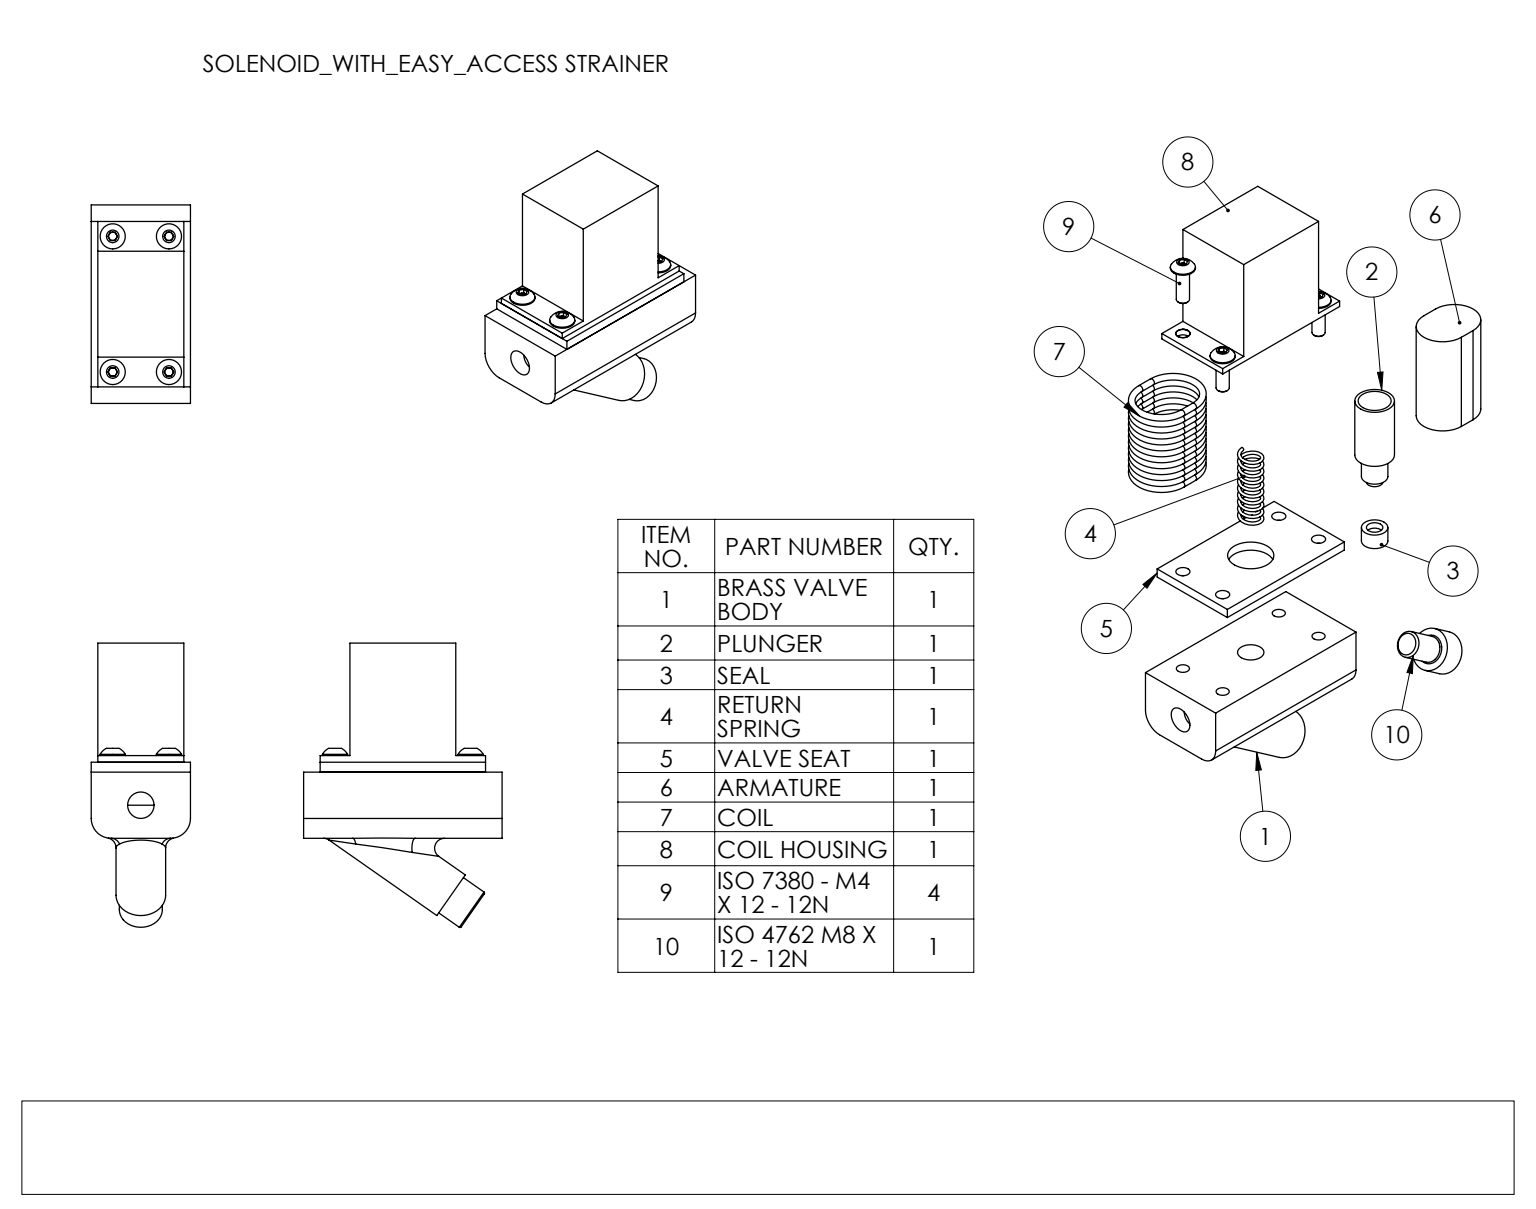
ISO-10303-21;
HEADER;
FILE_DESCRIPTION (('STEP AP214'),
    '1' );
FILE_NAME ('MAS-178',
    '2026-10-25T16:39:07',
    ( '' ),
    ( '' ),
    'SwSTEP 2.0',
    'SolidWorks 2026',
    '' );
FILE_SCHEMA (( 'AUTOMOTIVE_DESIGN' ));
ENDSEC;

DATA;
#1 = CARTESIAN_POINT ( 'NONE',  ( 1.444289557195957086, 32.75319992234354061, -4.262301884875733471 ) ) ;
#2 = CARTESIAN_POINT ( 'NONE',  ( 2.000000000000004441, -20.45500799277048287, -10.97077568596606056 ) ) ;
#3 = EDGE_LOOP ( 'NONE', ( #1646, #9949, #917, #16022, #4902 ) ) ;
#4 = CIRCLE ( 'NONE', #8561, 2.499999999999999556 ) ;
#5 = DIRECTION ( 'NONE',  ( -0.000000000000000000, 1.000000000000000000, -0.000000000000000000 ) ) ;
#6 = CARTESIAN_POINT ( 'NONE',  ( 3.518350579753631191, 24.37180007765648071, 1.080741659609802285 ) ) ;
#7 = CARTESIAN_POINT ( 'NONE',  ( 9.986002763741593569, -9.918550557884699970, 7.302443594976057106 ) ) ;
#8 = CARTESIAN_POINT ( 'NONE',  ( 2.121784821875004390, -19.91118585227123816, -10.56187548683408828 ) ) ;
#9 = CARTESIAN_POINT ( 'NONE',  ( -1.336863392178478716, 22.49680007765647360, 4.297206761780677731 ) ) ;
#10 = CARTESIAN_POINT ( 'NONE',  ( 3.579096709490575479E-14, -22.86967407583208711, -1.406012196336041020 ) ) ;
#11 = LINE ( 'NONE', #8170, #4109 ) ;
#12 = ORIENTED_EDGE ( 'NONE', *, *, #11357, .T. ) ;
#13 = VERTEX_POINT ( 'NONE', #16013 ) ;
#14 = CARTESIAN_POINT ( 'NONE',  ( -2.115076519116362519, 25.12180007765647360, 3.012182706137107147 ) ) ;
#15 = EDGE_CURVE ( 'NONE', #13968, #17116, #3305, .T. ) ;
#16 = FACE_OUTER_BOUND ( 'NONE', #9142, .T. ) ;
#17 = CARTESIAN_POINT ( 'NONE',  ( 0.000000000000000000, 0.000000000000000000, 4.000000000000000000 ) ) ;
#18 = FACE_OUTER_BOUND ( 'NONE', #18196, .T. ) ;
#19 = EDGE_LOOP ( 'NONE', ( #11268, #10681 ) ) ;
#20 = AXIS2_PLACEMENT_3D ( 'NONE', #7890, #15986, #13371 ) ;
#21 = CARTESIAN_POINT ( 'NONE',  ( 3.518350579753605434, 18.12819992234353705, -1.080741659609877114 ) ) ;
#22 = CARTESIAN_POINT ( 'NONE',  ( 4.243569643750000786, -23.22272928460757413, -8.884014471503119736 ) ) ;
#23 = CARTESIAN_POINT ( 'NONE',  ( -2.798362969681365886, 35.24680007765648071, 2.102939460078824929 ) ) ;
#24 = CARTESIAN_POINT ( 'NONE',  ( 0.05938372350920109732, 27.62819992234353705, -3.680117784833935701 ) ) ;
#25 = DIRECTION ( 'NONE',  ( 0.000000000000000000, 0.000000000000000000, -1.000000000000000000 ) ) ;
#26 = CYLINDRICAL_SURFACE ( 'NONE', #5055, 6.500000000000000000 ) ;
#27 = CARTESIAN_POINT ( 'NONE',  ( -5.330712181944245322E-15, -26.55907985683728967, -5.105836667743160362 ) ) ;
#28 = CIRCLE ( 'NONE', #5350, 0.9999999999999991118 ) ;
#29 = CARTESIAN_POINT ( 'NONE',  ( 10.00000000000000355, 23.19999999999999574, 2.499999999999996891 ) ) ;
#30 = ADVANCED_FACE ( 'NONE', ( #12002 ), #4961, .F. ) ;
#31 = EDGE_CURVE ( 'NONE', #634, #10845, #10430, .T. ) ;
#32 = DIRECTION ( 'NONE',  ( 1.000000000000000000, 0.000000000000000000, 0.000000000000000000 ) ) ;
#33 = ADVANCED_FACE ( 'NONE', ( #17875 ), #13949, .T. ) ;
#34 = DIRECTION ( 'NONE',  ( -0.000000000000000000, -1.000000000000000000, -0.000000000000000000 ) ) ;
#35 = CARTESIAN_POINT ( 'NONE',  ( -4.243569643750000786, -19.99636183013295820, -4.276284222377527477 ) ) ;
#36 = DIRECTION ( 'NONE',  ( 0.000000000000000000, 0.000000000000000000, 1.000000000000000000 ) ) ;
#37 = SURFACE_STYLE_USAGE ( .BOTH. , #13947 ) ;
#38 = ORIENTED_EDGE ( 'NONE', *, *, #726, .T. ) ;
#39 = CARTESIAN_POINT ( 'NONE',  ( -2.518350579753611207, 21.87819992234354416, 0.7558219633769609480 ) ) ;
#40 = CYLINDRICAL_SURFACE ( 'NONE', #15087, 5.000000000000000000 ) ;
#41 = CARTESIAN_POINT ( 'NONE',  ( -11.99999999999999822, 48.00000000000000000, 15.00000000000000000 ) ) ;
#42 = STYLED_ITEM ( 'NONE', ( #4855 ), #12463 ) ;
#43 = FACE_OUTER_BOUND ( 'NONE', #17351, .T. ) ;
#44 = LINE ( 'NONE', #5782, #7268 ) ;
#45 = ORIENTED_EDGE ( 'NONE', *, *, #5518, .T. ) ;
#46 = CARTESIAN_POINT ( 'NONE',  ( -4.243569643750000786, -20.54484429739364515, -5.059598364728879361 ) ) ;
#47 = CARTESIAN_POINT ( 'NONE',  ( 0.05938372350927906274, 32.37180007765647360, 3.680117784833935701 ) ) ;
#48 = DIRECTION ( 'NONE',  ( 0.000000000000000000, 0.000000000000000000, -1.000000000000000000 ) ) ;
#49 = CARTESIAN_POINT ( 'NONE',  ( -2.121784821874996396, -23.22358977219849407, -15.29247854260303718 ) ) ;
#50 =( BOUNDED_CURVE ( )  B_SPLINE_CURVE ( 2, ( #611, #13389, #3391, #8936, #1817, #3112, #11902, #16101, #955 ),
 .UNSPECIFIED., .F., .F. ) 
 B_SPLINE_CURVE_WITH_KNOTS ( ( 3, 2, 2, 2, 3 ),
 ( 0.3879310344827586188, 0.3908045977011494476, 0.3965517241379310498, 0.4022988505747126520, 0.4051724137931034808 ),
 .UNSPECIFIED. ) 
 CURVE ( )  GEOMETRIC_REPRESENTATION_ITEM ( )  RATIONAL_B_SPLINE_CURVE ( ( 0.9330127018922194093, 0.9330127018922194093, 1.000000000000000000, 0.8660254037844387076, 1.000000000000000000, 0.8660254037844387076, 1.000000000000000000, 0.9330127018922187432, 0.9330127018922194093 ) ) 
 REPRESENTATION_ITEM ( '' )  );
#51 = DIRECTION ( 'NONE',  ( 1.000000000000000000, 0.000000000000000000, -4.336808689942021680E-16 ) ) ;
#52 = PRESENTATION_LAYER_ASSIGNMENT (  '', '', ( #2717 ) ) ;
#53 = DIRECTION ( 'NONE',  ( -0.000000000000000000, -0.5735764363510414965, -0.8191520442889950182 ) ) ;
#54 = CARTESIAN_POINT ( 'NONE',  ( 4.243569643750003451, -22.48482328119956009, -12.10166559521431573 ) ) ;
#55 = ORIENTED_EDGE ( 'NONE', *, *, #17293, .T. ) ;
#56 = DIRECTION ( 'NONE',  ( -3.373073425510457965E-16, 0.000000000000000000, -1.000000000000000000 ) ) ;
#57 = CARTESIAN_POINT ( 'NONE',  ( -1.999999999999996225, -18.15353254261686899, -7.683928109263233885 ) ) ;
#58 = CARTESIAN_POINT ( 'NONE',  ( 2.055738996568313048, 21.99680007765648426, 1.423772053676023441 ) ) ;
#59 = EDGE_LOOP ( 'NONE', ( #6650, #2880, #2585, #4940 ) ) ;
#60 = DIRECTION ( 'NONE',  ( -1.000000000000000000, 0.000000000000000000, 4.336808689942021680E-16 ) ) ;
#61 = VECTOR ( 'NONE', #15535, 1000.000000000000000 ) ;
#62 = EDGE_CURVE ( 'NONE', #4590, #2518, #8726, .T. ) ;
#63 = AXIS2_PLACEMENT_3D ( 'NONE', #11586, #12802, #2984 ) ;
#64 = CARTESIAN_POINT ( 'NONE',  ( 3.999999999999996447, -25.24891187463481046, -7.751385191667569785 ) ) ;
#65 = CARTESIAN_POINT ( 'NONE',  ( 0.8262555684460829442, 37.75319992234354771, -2.360188852285421302 ) ) ;
#66 = EDGE_LOOP ( 'NONE', ( #4791, #2042, #17064, #10532, #9168 ) ) ;
#67 = CARTESIAN_POINT ( 'NONE',  ( 2.121784821875004390, -20.71777771588989125, -11.71380804911548701 ) ) ;
#68 = CARTESIAN_POINT ( 'NONE',  ( -4.000000000000000888, -26.36843755307278414, -13.37655146490396341 ) ) ;
#69 = CARTESIAN_POINT ( 'NONE',  ( 4.518350579753633411, 31.87180007765647716, 1.405661355842698468 ) ) ;
#70 = EDGE_LOOP ( 'NONE', ( #14455, #11089, #12235, #9427, #6688 ) ) ;
#71 = DIRECTION ( 'NONE',  ( 1.000000000000000000, 0.000000000000000000, 0.000000000000000000 ) ) ;
#72 = CARTESIAN_POINT ( 'NONE',  ( 1.071796769724485232, -23.37436616782919074, -2.126787201540221162 ) ) ;
#73 = DIRECTION ( 'NONE',  ( -0.000000000000000000, 1.000000000000000000, -0.000000000000000000 ) ) ;
#74 = AXIS2_PLACEMENT_3D ( 'NONE', #11287, #9899, #17353 ) ;
#75 = DIRECTION ( 'NONE',  ( -0.000000000000000000, 1.000000000000000000, -0.000000000000000000 ) ) ;
#76 =( GEOMETRIC_REPRESENTATION_CONTEXT ( 3 ) GLOBAL_UNCERTAINTY_ASSIGNED_CONTEXT ( ( #9698 ) ) GLOBAL_UNIT_ASSIGNED_CONTEXT ( ( #9720, #5466, #12594 ) ) REPRESENTATION_CONTEXT ( 'NONE', 'WORKASPACE' ) );
#77 = CARTESIAN_POINT ( 'NONE',  ( 10.00000000000000000, 34.19999999999999574, -2.500000000000003109 ) ) ;
#78 = CARTESIAN_POINT ( 'NONE',  ( 4.243569643749996345, -23.73478956620236957, -5.343822230353133307 ) ) ;
#79 = ADVANCED_FACE ( 'NONE', ( #10984 ), #15448, .F. ) ;
#80 = ORIENTED_EDGE ( 'NONE', *, *, #14785, .F. ) ;
#81 = CARTESIAN_POINT ( 'NONE',  ( 3.885274725274725949, -4.336808689942017736E-16, 0.000000000000000000 ) ) ;
#82 = ORIENTED_EDGE ( 'NONE', *, *, #14672, .T. ) ;
#83 = ORIENTED_EDGE ( 'NONE', *, *, #13971, .F. ) ;
#84 = DIRECTION ( 'NONE',  ( -0.000000000000000000, 1.000000000000000000, -0.000000000000000000 ) ) ;
#85 = EDGE_CURVE ( 'NONE', #1006, #3919, #10004, .T. ) ;
#86 = LINE ( 'NONE', #7211, #12515 ) ;
#87 = CARTESIAN_POINT ( 'NONE',  ( 4.499999999999999112, 18.25319992234354771, 0.05647727720528474687 ) ) ;
#88 = CARTESIAN_POINT ( 'NONE',  ( -2.115076519116425580, 27.37819992234354771, -3.012182706137063182 ) ) ;
#89 = CARTESIAN_POINT ( 'NONE',  ( 3.999999999999996447, -27.63642379165096941, -11.16110557702727668 ) ) ;
#90 = CARTESIAN_POINT ( 'NONE',  ( -1.593127413382998459, 35.87180007765648071, -2.091722143975139669 ) ) ;
#91 = AXIS2_PLACEMENT_3D ( 'NONE', #15450, #198, #8713 ) ;
#92 = CARTESIAN_POINT ( 'NONE',  ( 2.733110507866328920, 36.12819992234354771, 3.862833514489095510 ) ) ;
#93 = CARTESIAN_POINT ( 'NONE',  ( 1.999999999999994449, -26.47440569391090648, -7.488412793402255296 ) ) ;
#94 = VERTEX_POINT ( 'NONE', #4123 ) ;
#95 = CARTESIAN_POINT ( 'NONE',  ( 0.000000000000000000, 5.977523610840987267, 32.81826849749789687 ) ) ;
#96 = CARTESIAN_POINT ( 'NONE',  ( 2.798362969681366330, 18.99680007765648071, -2.102939460078824929 ) ) ;
#97 = CARTESIAN_POINT ( 'NONE',  ( 9.570744302495992173, -9.974069202854233041, -0.5947597794661263482 ) ) ;
#98 = CARTESIAN_POINT ( 'NONE',  ( -4.243569643749998122, -21.36634923031502353, -10.50431910885077791 ) ) ;
#99 = CARTESIAN_POINT ( 'NONE',  ( 4.518350579753633411, 21.87180007765647360, 1.405661355842698468 ) ) ;
#100 = AXIS2_PLACEMENT_3D ( 'NONE', #14724, #10710, #2117 ) ;
#101 = CARTESIAN_POINT ( 'NONE',  ( 1.071796769724504328, -22.85814737511324424, -1.389550361680131685 ) ) ;
#102 = CARTESIAN_POINT ( 'NONE',  ( 4.000000000000000888, -19.98022999250811793, -4.253245570628513939 ) ) ;
#103 = EDGE_CURVE ( 'NONE', #5353, #12502, #9927, .T. ) ;
#104 = ORIENTED_EDGE ( 'NONE', *, *, #5539, .F. ) ;
#105 = EDGE_LOOP ( 'NONE', ( #9337, #11121, #10529, #10635, #17849 ) ) ;
#106 = CARTESIAN_POINT ( 'NONE',  ( -3.500000000000000444, 22.99680007765647716, 0.05647727720536892260 ) ) ;
#107 = CARTESIAN_POINT ( 'NONE',  ( 0.000000000000000000, 29.79999999999999716, 2.500000000000000000 ) ) ;
#108 = CYLINDRICAL_SURFACE ( 'NONE', #4806, 0.9999999999999991118 ) ;
#109 =( LENGTH_UNIT ( ) NAMED_UNIT ( * ) SI_UNIT ( .MILLI., .METRE. ) );
#110 = EDGE_LOOP ( 'NONE', ( #10063, #7100, #15621, #8878 ) ) ;
#111 = CARTESIAN_POINT ( 'NONE',  ( -3.481649420246394122, 22.12819992234353705, -1.193696214020467883 ) ) ;
#112 = CARTESIAN_POINT ( 'NONE',  ( 4.243569643750000786, -23.48083868096554028, -9.252632891433169249 ) ) ;
#113 = CARTESIAN_POINT ( 'NONE',  ( 2.211161402132902243, 37.12180007765645939, 2.942372952327172442 ) ) ;
#114 = CARTESIAN_POINT ( 'NONE',  ( 1.027846397803612311, 36.25319992234354771, 3.346150245485499219 ) ) ;
#115 = CARTESIAN_POINT ( 'NONE',  ( 1.300000000000000044, -1.443375672974064328, 2.168404344971008868E-16 ) ) ;
#116 = CARTESIAN_POINT ( 'NONE',  ( 4.898587196589413815E-16, 2.700915433685006750, 35.11257424290206330 ) ) ;
#117 = VECTOR ( 'NONE', #8182, 1000.000000000000000 ) ;
#118 = CARTESIAN_POINT ( 'NONE',  ( -2.121784821874996396, -19.38421250137371388, -9.809279546143578443 ) ) ;
#119 = CARTESIAN_POINT ( 'NONE',  ( -2.526502195916607629, -15.31622431266957207, -9.916727303590223030 ) ) ;
#120 = CARTESIAN_POINT ( 'NONE',  ( -5.577813053751546416E-15, -24.16022105762193206, -3.249104295986281699 ) ) ;
#121 = CARTESIAN_POINT ( 'NONE',  ( 8.500000000000001776, 13.00000000000000178, -20.49999999999999645 ) ) ;
#122 = CARTESIAN_POINT ( 'NONE',  ( 4.243569643749996345, -22.92819770258371292, -4.191889668071731911 ) ) ;
#123 = CARTESIAN_POINT ( 'NONE',  ( 1.071796769724485454, -21.36111765121935235, -13.19914471043622228 ) ) ;
#124 =( NAMED_UNIT ( * ) SI_UNIT ( $, .STERADIAN. ) SOLID_ANGLE_UNIT ( ) );
#125 = ORIENTED_EDGE ( 'NONE', *, *, #9998, .T. ) ;
#126 = CARTESIAN_POINT ( 'NONE',  ( -0.05938372350921170689, 21.37819992234354416, 2.628655560595669183 ) ) ;
#127 = CARTESIAN_POINT ( 'NONE',  ( -5.577813053751546416E-15, -25.38624068961733826, -5.000041789647243107 ) ) ;
#128 = DIRECTION ( 'NONE',  ( -1.000000000000000000, -0.000000000000000000, -0.000000000000000000 ) ) ;
#129 = CYLINDRICAL_SURFACE ( 'NONE', #10158, 6.000000000000000000 ) ;
#130 = DIRECTION ( 'NONE',  ( -1.000000000000000000, 0.000000000000000000, -0.000000000000000000 ) ) ;
#131 = EDGE_CURVE ( 'NONE', #9627, #9963, #4373, .T. ) ;
#132 = ORIENTED_EDGE ( 'NONE', *, *, #13174, .F. ) ;
#133 = CARTESIAN_POINT ( 'NONE',  ( 2.121784821875004390, -17.62046495959427261, -7.290387009954915953 ) ) ;
#134 = CARTESIAN_POINT ( 'NONE',  ( -0.05938372350927861171, 36.12180007765648782, -3.680117784833935701 ) ) ;
#135 = CARTESIAN_POINT ( 'NONE',  ( -4.000000000000000888, -19.85117529432912775, -4.068936360663492735 ) ) ;
#136 = ADVANCED_FACE ( 'NONE', ( #2566 ), #16663, .T. ) ;
#137 = EDGE_CURVE ( 'NONE', #3649, #894, #1162, .T. ) ;
#138 = CARTESIAN_POINT ( 'NONE',  ( -4.243569643749998122, -23.17311500482080433, -13.08464804836111206 ) ) ;
#139 = CARTESIAN_POINT ( 'NONE',  ( 9.000000000000005329, 36.39999999999999147, 2.499999999999997335 ) ) ;
#140 = VECTOR ( 'NONE', #8743, 1000.000000000000000 ) ;
#141 = EDGE_CURVE ( 'NONE', #15889, #18202, #16275, .T. ) ;
#142 = DIRECTION ( 'NONE',  ( 0.000000000000000000, 0.000000000000000000, -1.000000000000000000 ) ) ;
#143 = LINE ( 'NONE', #14051, #16513 ) ;
#144 = CARTESIAN_POINT ( 'NONE',  ( 4.243569643749996345, -26.79983864795324422, -9.721165967022450616 ) ) ;
#145 = LINE ( 'NONE', #7551, #15141 ) ;
#146 = CARTESIAN_POINT ( 'NONE',  ( -1.999999999999996225, -17.37920435354295989, -6.578072849473089789 ) ) ;
#147 = CARTESIAN_POINT ( 'NONE',  ( 1.593127413382998903, 24.62180007765647716, 2.091722143975139669 ) ) ;
#148 = ORIENTED_EDGE ( 'NONE', *, *, #10556, .T. ) ;
#149 = CARTESIAN_POINT ( 'NONE',  ( 2.115076519116362963, 23.87180007765647360, -3.012182706137107591 ) ) ;
#150 = EDGE_CURVE ( 'NONE', #12707, #13230, #14438, .T. ) ;
#151 = CARTESIAN_POINT ( 'NONE',  ( 0.000000000000000000, 5.977523610840987267, 32.81826849749789687 ) ) ;
#152 = CARTESIAN_POINT ( 'NONE',  ( 0.000000000000000000, 0.000000000000000000, 0.000000000000000000 ) ) ;
#153 = DIRECTION ( 'NONE',  ( 0.000000000000000000, 0.000000000000000000, 1.000000000000000000 ) ) ;
#154 = CARTESIAN_POINT ( 'NONE',  ( -0.05938372350921170689, 33.87819992234354061, 2.628655560595669183 ) ) ;
#155 = PRODUCT_DEFINITION ( 'UNKNOWN', '', #10424, #5149 ) ;
#156 = VERTEX_POINT ( 'NONE', #15172 ) ;
#157 = CARTESIAN_POINT ( 'NONE',  ( -2.121784821874996396, -21.44908767223746437, -12.75822690558396033 ) ) ;
#158 = CARTESIAN_POINT ( 'NONE',  ( -3.607379964056306676, 35.24680007765647360, 2.690724712371306282 ) ) ;
#159 = VERTEX_POINT ( 'NONE', #2476 ) ;
#160 = VECTOR ( 'NONE', #10107, 1000.000000000000000 ) ;
#161 = CARTESIAN_POINT ( 'NONE',  ( 3.999999999999995559, 2.343145750507624747, 2.343145750507618086 ) ) ;
#162 = CARTESIAN_POINT ( 'NONE',  ( -5.577813053751546416E-15, -26.16056887869124381, -6.105897049437384538 ) ) ;
#163 = CARTESIAN_POINT ( 'NONE',  ( 1.071796769724485232, -25.37471398889850605, -4.983579954991325778 ) ) ;
#164 = CARTESIAN_POINT ( 'NONE',  ( -5.577813053751546416E-15, -29.06429958842333505, -10.25285427465718868 ) ) ;
#165 = LINE ( 'NONE', #4426, #8792 ) ;
#166 = CARTESIAN_POINT ( 'NONE',  ( 2.121784821874994176, -23.98544242790896774, -3.566046559362932467 ) ) ;
#167 = ORIENTED_EDGE ( 'NONE', *, *, #2613, .T. ) ;
#168 = CARTESIAN_POINT ( 'NONE',  ( 9.000000000000001776, 20.99999999999999289, -2.500000000000002665 ) ) ;
#169 = EDGE_LOOP ( 'NONE', ( #15590, #17525, #15025, #11757 ) ) ;
#170 = ORIENTED_EDGE ( 'NONE', *, *, #9208, .T. ) ;
#171 = CYLINDRICAL_SURFACE ( 'NONE', #7169, 2.000000000000001776 ) ;
#172 = LINE ( 'NONE', #7581, #17268 ) ;
#173 = CARTESIAN_POINT ( 'NONE',  ( 2.733110507866328920, 21.12819992234354416, 3.862833514489095510 ) ) ;
#174 = CARTESIAN_POINT ( 'NONE',  ( -2.211161402132838738, 26.62819992234354416, 2.942372952327218183 ) ) ;
#175 = AXIS2_PLACEMENT_3D ( 'NONE', #15900, #11338, #4486 ) ;
#176 = CARTESIAN_POINT ( 'NONE',  ( -1.989345975306426206, 40.24680007765648071, 1.515154207786343799 ) ) ;
#177 = VERTEX_POINT ( 'NONE', #8106 ) ;
#178 = CARTESIAN_POINT ( 'NONE',  ( 0.05938372350919016857, 32.62819992234354771, -4.731580009072201776 ) ) ;
#179 = CARTESIAN_POINT ( 'NONE',  ( -3.999999999999997335, -21.07824655387797819, -9.847693641197304615 ) ) ;
#180 = ORIENTED_EDGE ( 'NONE', *, *, #14181, .F. ) ;
#181 = DIRECTION ( 'NONE',  ( 1.000000000000000000, 0.000000000000000000, 0.000000000000000000 ) ) ;
#182 = CARTESIAN_POINT ( 'NONE',  ( -2.798362969681365886, 30.24680007765648071, 2.102939460078824929 ) ) ;
#183 = CLOSED_SHELL ( 'NONE', ( #8623, #12070, #5801, #4336, #16789, #13518, #7804, #15959, #10685, #12852, #17802, #16024, #17150, #1736, #8963, #16034, #14996, #8741, #15227, #15885, #6061, #555, #6136, #15606, #14685, #7463, #6386 ) ) ;
#184 = CARTESIAN_POINT ( 'NONE',  ( -9.604277560388482016, -9.971758527880211886, 12.06915245473052778 ) ) ;
#185 = CARTESIAN_POINT ( 'NONE',  ( 4.243569643750003451, -19.90372931761987019, -8.415481395913838369 ) ) ;
#186 = CIRCLE ( 'NONE', #5222, 0.9999999999999991118 ) ;
#187 = CARTESIAN_POINT ( 'NONE',  ( 4.518350579753633411, 34.37180007765647360, 1.405661355842698468 ) ) ;
#188 = DIRECTION ( 'NONE',  ( -0.000000000000000000, -1.000000000000000000, -0.000000000000000000 ) ) ;
#189 = ORIENTED_EDGE ( 'NONE', *, *, #16096, .T. ) ;
#190 = ORIENTED_EDGE ( 'NONE', *, *, #1172, .T. ) ;
#191 = CARTESIAN_POINT ( 'NONE',  ( -2.115076519116362519, 27.62180007765648071, 3.012182706137107147 ) ) ;
#192 = CARTESIAN_POINT ( 'NONE',  ( 4.000000000000000000, 3.518949890710770134, -4.119968255444916849E-15 ) ) ;
#193 = DIRECTION ( 'NONE',  ( 0.000000000000000000, 0.000000000000000000, -1.000000000000000000 ) ) ;
#194 = CARTESIAN_POINT ( 'NONE',  ( 1.533898589781675205E-14, -27.70922525683905846, -8.317607569017670954 ) ) ;
#195 = FILL_AREA_STYLE ('',( #580 ) ) ;
#196 = VERTEX_POINT ( 'NONE', #13765 ) ;
#197 = CARTESIAN_POINT ( 'NONE',  ( 2.115076519116426024, 21.12819992234353705, 3.012182706137062294 ) ) ;
#198 = DIRECTION ( 'NONE',  ( -1.000000000000000000, -0.000000000000000000, -0.000000000000000000 ) ) ;
#199 = CARTESIAN_POINT ( 'NONE',  ( 4.730628863548789710E-15, -18.62809540513275408, -10.86517747810410306 ) ) ;
#200 = CARTESIAN_POINT ( 'NONE',  ( -3.481649420246369697, 37.87180007765648071, 1.193696214020542490 ) ) ;
#201 = EDGE_CURVE ( 'NONE', #2949, #3217, #16754, .T. ) ;
#202 = CARTESIAN_POINT ( 'NONE',  ( -0.05938372350920063936, 31.37819992234354416, 3.680117784833935701 ) ) ;
#203 = FACE_OUTER_BOUND ( 'NONE', #11493, .T. ) ;
#204 = VECTOR ( 'NONE', #11238, 1000.000000000000227 ) ;
#205 = DIRECTION ( 'NONE',  ( 0.000000000000000000, 0.8191520442889952403, -0.5735764363510413855 ) ) ;
#206 = CARTESIAN_POINT ( 'NONE',  ( -4.243569643750005227, -25.11137301344485451, -7.309787136646725081 ) ) ;
#207 = EDGE_CURVE ( 'NONE', #12141, #13551, #11942, .T. ) ;
#208 = CYLINDRICAL_SURFACE ( 'NONE', #2997, 2.000000000000001776 ) ;
#209 = PRODUCT_DEFINITION_CONTEXT ( 'detailed design', #4162, 'design' ) ;
#210 = EDGE_CURVE ( 'NONE', #16170, #12849, #15356, .T. ) ;
#211 = CARTESIAN_POINT ( 'NONE',  ( -4.371749249414769167, -10.00000000000000178, -10.94697576041360954 ) ) ;
#212 = DIRECTION ( 'NONE',  ( 0.000000000000000000, 0.8191520442889952403, -0.5735764363510413855 ) ) ;
#213 = DIRECTION ( 'NONE',  ( 1.000000000000000000, 0.000000000000000000, 0.000000000000000000 ) ) ;
#214 = VECTOR ( 'NONE', #7659, 1000.000000000000000 ) ;
#215 = CARTESIAN_POINT ( 'NONE',  ( 4.730628863548789710E-15, -16.82132963062697684, -8.284848538593767131 ) ) ;
#216 = CARTESIAN_POINT ( 'NONE',  ( -1.086818808809129289, 15.00000000000000533, -3.240250934315705322 ) ) ;
#217 = CARTESIAN_POINT ( 'NONE',  ( 2.000000000000004441, -17.68033198262726913, -7.008127672724814516 ) ) ;
#218 = VERTEX_POINT ( 'NONE', #12642 ) ;
#219 = CARTESIAN_POINT ( 'NONE',  ( 0.8262555684460829442, 20.25319992234354771, -2.360188852285421302 ) ) ;
#220 = CARTESIAN_POINT ( 'NONE',  ( 4.243569643749996345, -28.60660442245902146, -12.30149490653278121 ) ) ;
#221 = DIRECTION ( 'NONE',  ( -1.000000000000000000, 0.000000000000000000, 0.000000000000000000 ) ) ;
#222 = CARTESIAN_POINT ( 'NONE',  ( -1.444289557196047014, 18.49680007765647360, -4.262301884875704161 ) ) ;
#223 = CARTESIAN_POINT ( 'NONE',  ( -8.999999999999996447, -10.00000000000000000, 15.14468620625656925 ) ) ;
#224 = DIRECTION ( 'NONE',  ( -6.162975822039154730E-33, 0.5735764363510414965, 0.8191520442889950182 ) ) ;
#225 = ADVANCED_FACE ( 'NONE', ( #14226 ), #13254, .T. ) ;
#226 = CLOSED_SHELL ( 'NONE', ( #8070, #9759, #11243, #8369, #10714, #5967, #5501, #385, #7224, #136 ) ) ;
#227 = ORIENTED_EDGE ( 'NONE', *, *, #6831, .F. ) ;
#228 = CARTESIAN_POINT ( 'NONE',  ( 2.121784821875004390, -17.36235556323629936, -6.921768590024867329 ) ) ;
#229 = CARTESIAN_POINT ( 'NONE',  ( -0.05938372350927861171, 31.12180007765647005, -3.680117784833935701 ) ) ;
#230 = CARTESIAN_POINT ( 'NONE',  ( 3.064182432158234271, -21.85725826261086624, -2.451265441397198153 ) ) ;
#231 = AXIS2_PLACEMENT_3D ( 'NONE', #14903, #8098, #17958 ) ;
#232 = CARTESIAN_POINT ( 'NONE',  ( 9.000000000000005329, 23.19999999999999574, 2.499999999999997335 ) ) ;
#233 = CARTESIAN_POINT ( 'NONE',  ( 4.243569643749997233, -27.57416683702714622, -10.82702122681259205 ) ) ;
#234 = CARTESIAN_POINT ( 'NONE',  ( 3.061616997868382648E-16, 3.000000000000000000, -2.499999999999999556 ) ) ;
#235 = CYLINDRICAL_SURFACE ( 'NONE', #4146, 4.000000000000000000 ) ;
#236 = DIRECTION ( 'NONE',  ( 0.000000000000000000, 0.8191520442889952403, -0.5735764363510413855 ) ) ;
#237 = CARTESIAN_POINT ( 'NONE',  ( -4.243569643750000786, -24.64233096457639505, -10.91141578111838584 ) ) ;
#238 = EDGE_CURVE ( 'NONE', #14275, #456, #5568, .T. ) ;
#239 = PLANE ( 'NONE',  #7419 ) ;
#240 = CARTESIAN_POINT ( 'NONE',  ( -5.279047395330986450E-15, -24.40900471032784935, -2.525555542035599288 ) ) ;
#241 = AXIS2_PLACEMENT_3D ( 'NONE', #5032, #10687, #16359 ) ;
#242 = CARTESIAN_POINT ( 'NONE',  ( 2.518350579753628971, 21.87180007765647360, 0.7558219633769073242 ) ) ;
#243 = CIRCLE ( 'NONE', #11190, 2.149999999999999023 ) ;
#244 = VERTEX_POINT ( 'NONE', #11334 ) ;
#245 = CARTESIAN_POINT ( 'NONE',  ( 0.05938372350927906967, 19.87180007765648071, 3.680117784833935701 ) ) ;
#246 = FACE_OUTER_BOUND ( 'NONE', #4639, .T. ) ;
#247 = DIRECTION ( 'NONE',  ( 0.000000000000000000, -1.000000000000000000, 0.000000000000000000 ) ) ;
#248 = CARTESIAN_POINT ( 'NONE',  ( 1.071796769724504328, -26.66526097068834034, -6.826672054641570675 ) ) ;
#249 = CARTESIAN_POINT ( 'NONE',  ( 0.7188294034286553114, 33.75319992234354771, 2.395093729190349130 ) ) ;
#250 = ORIENTED_EDGE ( 'NONE', *, *, #10800, .T. ) ;
#251 = CARTESIAN_POINT ( 'NONE',  ( 2.121784821874994176, -27.34086458056255964, -8.358086018453551702 ) ) ;
#252 = CARTESIAN_POINT ( 'NONE',  ( -2.733110507866247652, 32.62180007765647360, 3.862833514489154574 ) ) ;
#253 = ORIENTED_EDGE ( 'NONE', *, *, #12378, .T. ) ;
#254 =( GEOMETRIC_REPRESENTATION_CONTEXT ( 3 ) GLOBAL_UNCERTAINTY_ASSIGNED_CONTEXT ( ( #16629 ) ) GLOBAL_UNIT_ASSIGNED_CONTEXT ( ( #17586, #16356, #4937 ) ) REPRESENTATION_CONTEXT ( 'NONE', 'WORKASPACE' ) );
#255 = TOROIDAL_SURFACE ( 'NONE', #10616, 9.000000000000001776, 0.9999999999999991118 ) ;
#256 = CARTESIAN_POINT ( 'NONE',  ( 7.960204194457794491E-16, 43.00000000000000000, 6.499999999999999112 ) ) ;
#257 = CARTESIAN_POINT ( 'NONE',  ( 4.243569643750003451, -23.54952454117618288, -13.62221657742576397 ) ) ;
#258 = DIRECTION ( 'NONE',  ( 0.000000000000000000, 0.000000000000000000, 1.000000000000000000 ) ) ;
#259 = CYLINDRICAL_SURFACE ( 'NONE', #5612, 4.000000000000000000 ) ;
#260 = DIRECTION ( 'NONE',  ( -0.000000000000000000, -1.000000000000000000, 1.502314598737159031E-16 ) ) ;
#261 = CARTESIAN_POINT ( 'NONE',  ( -4.243569643749997233, -19.84995652671195998, -8.338685891761748792 ) ) ;
#262 = ORIENTED_EDGE ( 'NONE', *, *, #17903, .F. ) ;
#263 = ADVANCED_FACE ( 'NONE', ( #5958 ), #40, .F. ) ;
#264 = APPLICATION_CONTEXT ( 'automotive_design' ) ;
#265 = CARTESIAN_POINT ( 'NONE',  ( 8.673617379884035472E-15, 13.00000000000000178, 3.469446951953614189E-15 ) ) ;
#266 = DIRECTION ( 'NONE',  ( -0.000000000000000000, -1.000000000000000000, -0.000000000000000000 ) ) ;
#267 = ADVANCED_FACE ( 'NONE', ( #8551 ), #11828, .T. ) ;
#268 = EDGE_LOOP ( 'NONE', ( #17033, #4613, #7602, #12216 ) ) ;
#269 = VERTEX_POINT ( 'NONE', #1927 ) ;
#270 = CARTESIAN_POINT ( 'NONE',  ( 8.399999999999998579, 5.388445916248356971E-16, 4.400000000000002132 ) ) ;
#271 = CARTESIAN_POINT ( 'NONE',  ( 4.898587196589413815E-16, 2.700915433685006750, 35.11257424290206330 ) ) ;
#272 =( NAMED_UNIT ( * ) SI_UNIT ( $, .STERADIAN. ) SOLID_ANGLE_UNIT ( ) );
#273 = AXIS2_PLACEMENT_3D ( 'NONE', #9056, #14733, #2489 ) ;
#274 = CARTESIAN_POINT ( 'NONE',  ( 3.607379964056363075, 18.50319992234354416, 2.690724712371229010 ) ) ;
#275 = CARTESIAN_POINT ( 'NONE',  ( -2.864755990943222308, 26.75319992234354771, 2.011557305968548093 ) ) ;
#276 = AXIS2_PLACEMENT_3D ( 'NONE', #2238, #8890, #9173 ) ;
#277 = CARTESIAN_POINT ( 'NONE',  ( 2.518350579753628971, 34.37180007765647360, 0.7558219633769073242 ) ) ;
#278 = VERTEX_POINT ( 'NONE', #11912 ) ;
#279 = CARTESIAN_POINT ( 'NONE',  ( 2.829195390882724759, 35.37819992234354061, -3.793023760679264278 ) ) ;
#280 = CARTESIAN_POINT ( 'NONE',  ( -4.000000000000004441, -24.81872954737152170, -7.137021158450828295 ) ) ;
#281 = ORIENTED_EDGE ( 'NONE', *, *, #17408, .F. ) ;
#282 = DIRECTION ( 'NONE',  ( 0.000000000000000000, 0.000000000000000000, -1.000000000000000000 ) ) ;
#283 = AXIS2_PLACEMENT_3D ( 'NONE', #4294, #5954, #10212 ) ;
#284 = CARTESIAN_POINT ( 'NONE',  ( 2.864755990943265829, 31.99680007765647716, 2.011557305968487697 ) ) ;
#285 = CARTESIAN_POINT ( 'NONE',  ( -9.667409818421043965, -9.963321348641603237, 0.1620040674102612710 ) ) ;
#286 = CIRCLE ( 'NONE', #5316, 8.000000000000001776 ) ;
#287 = CARTESIAN_POINT ( 'NONE',  ( 4.243569643749997233, -22.92819770258370582, -4.191889668071731911 ) ) ;
#288 = AXIS2_PLACEMENT_3D ( 'NONE', #11365, #11189, #12854 ) ;
#289 = CARTESIAN_POINT ( 'NONE',  ( -2.733110507866247652, 27.62180007765647716, 3.862833514489154574 ) ) ;
#290 = DIRECTION ( 'NONE',  ( 0.000000000000000000, 0.000000000000000000, 1.000000000000000000 ) ) ;
#291 = ORIENTED_EDGE ( 'NONE', *, *, #12084, .T. ) ;
#292 = ORIENTED_EDGE ( 'NONE', *, *, #6272, .T. ) ;
#293 = CARTESIAN_POINT ( 'NONE',  ( 3.518350579753631191, 24.37180007765648071, 1.080741659609802285 ) ) ;
#294 = FACE_OUTER_BOUND ( 'NONE', #4878, .T. ) ;
#295 =( NAMED_UNIT ( * ) PLANE_ANGLE_UNIT ( ) SI_UNIT ( $, .RADIAN. ) );
#296 = CARTESIAN_POINT ( 'NONE',  ( -1.734723475976807094E-15, 38.59999999999999432, -2.500000000000000000 ) ) ;
#297 = VERTEX_POINT ( 'NONE', #12091 ) ;
#298 = CARTESIAN_POINT ( 'NONE',  ( -1.027846397803611866, 20.00319992234354416, -3.346150245485499219 ) ) ;
#299 = CARTESIAN_POINT ( 'NONE',  ( -1.071796769724494114, -29.59204508185809956, -11.00655294917319971 ) ) ;
#300 = CARTESIAN_POINT ( 'NONE',  ( 4.730628863548789710E-15, -19.14431419784869348, -11.60241431796419853 ) ) ;
#301 = CARTESIAN_POINT ( 'NONE',  ( 2.055738996568313048, 16.99680007765648071, 1.423772053676023441 ) ) ;
#302 = AXIS2_PLACEMENT_3D ( 'NONE', #7360, #4404, #10044 ) ;
#303 = CARTESIAN_POINT ( 'NONE',  ( 2.115076519116426024, 36.12819992234355482, 3.012182706137062294 ) ) ;
#304 = CARTESIAN_POINT ( 'NONE',  ( 8.000000000000001776, 16.59999999999999787, -2.500000000000002220 ) ) ;
#305 = CARTESIAN_POINT ( 'NONE',  ( -4.000000000000000888, -27.07823839235225094, -14.39025211870482934 ) ) ;
#306 = CARTESIAN_POINT ( 'NONE',  ( 4.243569643750003451, -20.19410238852258743, -8.830177118335141628 ) ) ;
#307 = DIRECTION ( 'NONE',  ( -0.000000000000000000, -0.5735764363510414965, -0.8191520442889950182 ) ) ;
#308 = CARTESIAN_POINT ( 'NONE',  ( -4.193264170084745501, -10.00000000000000178, -2.677076674081568797 ) ) ;
#309 = AXIS2_PLACEMENT_3D ( 'NONE', #1703, #12902, #17104 ) ;
#310 = CARTESIAN_POINT ( 'NONE',  ( 3.061616997868382648E-16, 3.000000000000000000, 2.499999999999999556 ) ) ;
#311 = DIRECTION ( 'NONE',  ( 1.000000000000000000, 0.000000000000000000, -4.336808689942021680E-16 ) ) ;
#312 = ORIENTED_EDGE ( 'NONE', *, *, #6152, .T. ) ;
#313 = CARTESIAN_POINT ( 'NONE',  ( -5.330712181944245322E-15, -24.20383161507082193, -1.742193585881474771 ) ) ;
#314 = EDGE_CURVE ( 'NONE', #17692, #15689, #18053, .T. ) ;
#315 = FACE_OUTER_BOUND ( 'NONE', #13052, .T. ) ;
#316 = DIRECTION ( 'NONE',  ( 0.000000000000000000, 0.000000000000000000, 1.000000000000000000 ) ) ;
#317 = VERTEX_POINT ( 'NONE', #16194 ) ;
#318 = CARTESIAN_POINT ( 'NONE',  ( 0.8262555684460829442, 17.75319992234354061, -2.360188852285421302 ) ) ;
#319 = EDGE_CURVE ( 'NONE', #18210, #10649, #7063, .T. ) ;
#320 = CARTESIAN_POINT ( 'NONE',  ( 2.121784821874994176, -29.88969486959749844, -11.99819291526277532 ) ) ;
#321 = LINE ( 'NONE', #17400, #16399 ) ;
#322 = CARTESIAN_POINT ( 'NONE',  ( -1.336863392178478716, 17.49680007765647716, 4.297206761780677731 ) ) ;
#323 = CARTESIAN_POINT ( 'NONE',  ( 7.347880794884120722E-16, 13.00000000000000178, -6.000000000000000888 ) ) ;
#324 = CARTESIAN_POINT ( 'NONE',  ( 3.820650143297091184, -10.00000000000057376, -3.109998371641698345 ) ) ;
#325 = ORIENTED_EDGE ( 'NONE', *, *, #7933, .F. ) ;
#326 = CARTESIAN_POINT ( 'NONE',  ( -2.121784821874996396, -17.57744672686793308, -7.228950606633243403 ) ) ;
#327 = CIRCLE ( 'NONE', #8019, 0.9999999999999991118 ) ;
#328 = CARTESIAN_POINT ( 'NONE',  ( -2.864755990943265829, 38.24680007765647360, -2.011557305968488141 ) ) ;
#329 = CARTESIAN_POINT ( 'NONE',  ( 2.121784821874994176, -29.66384914778427628, -11.67565179782398310 ) ) ;
#330 =( BOUNDED_CURVE ( )  B_SPLINE_CURVE ( 2, ( #8971, #16213, #4605, #6375, #1755, #13228, #14645, #544, #6189 ),
 .UNSPECIFIED., .F., .T. ) 
 B_SPLINE_CURVE_WITH_KNOTS ( ( 3, 2, 2, 2, 3 ),
 ( 0.2844827586206896686, 0.2873563218390804419, 0.2931034482758620441, 0.2988505747126437018, 0.3017241379310345306 ),
 .UNSPECIFIED. ) 
 CURVE ( )  GEOMETRIC_REPRESENTATION_ITEM ( )  RATIONAL_B_SPLINE_CURVE ( ( 0.9330127018922194093, 0.9330127018922200755, 1.000000000000000000, 0.8660254037844387076, 1.000000000000000000, 0.8660254037844387076, 1.000000000000000000, 0.9330127018922187432, 0.9330127018922194093 ) ) 
 REPRESENTATION_ITEM ( '' )  );
#331 = PLANE ( 'NONE',  #16743 ) ;
#332 = CARTESIAN_POINT ( 'NONE',  ( 4.730628863548789710E-15, -20.95107997235447073, -14.18274325747453268 ) ) ;
#333 = LINE ( 'NONE', #8939, #3459 ) ;
#334 = DIRECTION ( 'NONE',  ( 0.000000000000000000, 1.000000000000000000, 0.000000000000000000 ) ) ;
#335 = DIRECTION ( 'NONE',  ( 0.000000000000000000, 0.000000000000000000, 1.000000000000000000 ) ) ;
#336 = CARTESIAN_POINT ( 'NONE',  ( 4.243569643750000786, -24.77138566275538523, -11.09572499108340793 ) ) ;
#337 = EDGE_CURVE ( 'NONE', #1667, #17584, #9315, .T. ) ;
#338 = CARTESIAN_POINT ( 'NONE',  ( -8.000000000000003553, 20.99999999999999289, -2.500000000000001776 ) ) ;
#339 = CARTESIAN_POINT ( 'NONE',  ( -3.999999999999997335, -18.81978933645070384, -6.622282467816152263 ) ) ;
#340 =( GEOMETRIC_REPRESENTATION_CONTEXT ( 3 ) GLOBAL_UNCERTAINTY_ASSIGNED_CONTEXT ( ( #12516 ) ) GLOBAL_UNIT_ASSIGNED_CONTEXT ( ( #1395, #8421, #14269 ) ) REPRESENTATION_CONTEXT ( 'NONE', 'WORKASPACE' ) );
#341 = CARTESIAN_POINT ( 'NONE',  ( 0.7188294034286049072, 26.24680007765647716, -2.395093729190366005 ) ) ;
#342 = EDGE_CURVE ( 'NONE', #5337, #15144, #10613, .T. ) ;
#343 = EDGE_LOOP ( 'NONE', ( #3432, #4004, #414, #10263 ) ) ;
#344 = CARTESIAN_POINT ( 'NONE',  ( 3.518350579753631191, 19.37180007765648071, 1.080741659609802729 ) ) ;
#345 = DIRECTION ( 'NONE',  ( 1.000000000000000000, 0.000000000000000000, 0.000000000000000000 ) ) ;
#346 = CARTESIAN_POINT ( 'NONE',  ( -8.500000000000007105, 17.19999999999999929, -20.49999999999999645 ) ) ;
#347 = DIRECTION ( 'NONE',  ( 0.000000000000000000, 0.000000000000000000, -1.000000000000000000 ) ) ;
#348 = CARTESIAN_POINT ( 'NONE',  ( -2.864755990943222308, 16.75319992234354416, 2.011557305968548093 ) ) ;
#349 = ORIENTED_EDGE ( 'NONE', *, *, #16662, .F. ) ;
#350 = CARTESIAN_POINT ( 'NONE',  ( 4.243569643749997233, -25.54155534070815392, -7.924151169863465682 ) ) ;
#351 = CARTESIAN_POINT ( 'NONE',  ( -1.336863392178478716, 32.49680007765647360, 4.297206761780677731 ) ) ;
#352 = ORIENTED_EDGE ( 'NONE', *, *, #16895, .T. ) ;
#353 = PLANE ( 'NONE',  #5705 ) ;
#354 = CARTESIAN_POINT ( 'NONE',  ( 1.300000000000000044, 0.000000000000000000, 0.000000000000000000 ) ) ;
#355 = CARTESIAN_POINT ( 'NONE',  ( -2.121784821875005722, -27.90010160600482081, -9.156759261635325942 ) ) ;
#356 = CARTESIAN_POINT ( 'NONE',  ( 0.000000000000000000, 13.00000000000000178, 0.000000000000000000 ) ) ;
#357 = CARTESIAN_POINT ( 'NONE',  ( -14.99999999999999645, 10.00000000000000000, -30.00000000000000000 ) ) ;
#358 = CARTESIAN_POINT ( 'NONE',  ( 3.999999999999996447, -24.47458368556090491, -6.645529931877427465 ) ) ;
#359 = CARTESIAN_POINT ( 'NONE',  ( -4.243569643749997233, -19.07562833763805088, -7.232830631971606472 ) ) ;
#360 = ORIENTED_EDGE ( 'NONE', *, *, #444, .T. ) ;
#361 = CIRCLE ( 'NONE', #2453, 1.610000000000000098 ) ;
#362 = DIRECTION ( 'NONE',  ( 0.000000000000000000, 0.8191520442889952403, -0.5735764363510413855 ) ) ;
#363 = ORIENTED_EDGE ( 'NONE', *, *, #10501, .T. ) ;
#364 = ORIENTED_EDGE ( 'NONE', *, *, #9762, .T. ) ;
#365 = CARTESIAN_POINT ( 'NONE',  ( -3.999999999999997335, -18.56167994009273059, -6.253664047886104527 ) ) ;
#366 = FACE_OUTER_BOUND ( 'NONE', #5608, .T. ) ;
#367 = AXIS2_PLACEMENT_3D ( 'NONE', #13212, #13030, #15828 ) ;
#368 = CARTESIAN_POINT ( 'NONE',  ( -3.607379964056363075, 24.75319992234354416, -2.690724712371229899 ) ) ;
#369 = CARTESIAN_POINT ( 'NONE',  ( 2.798362969681409851, 26.00319992234354771, 2.102939460078764977 ) ) ;
#370 = CARTESIAN_POINT ( 'NONE',  ( -2.518350579753611207, 19.37819992234354771, 0.7558219633769609480 ) ) ;
#371 = ORIENTED_EDGE ( 'NONE', *, *, #11937, .T. ) ;
#372 = CARTESIAN_POINT ( 'NONE',  ( -1.444289557195956863, 31.50319992234354416, 4.262301884875733471 ) ) ;
#373 = CARTESIAN_POINT ( 'NONE',  ( 4.713407268011036227E-15, -18.45518598442047420, -10.12789282444123451 ) ) ;
#374 = ORIENTED_EDGE ( 'NONE', *, *, #3443, .F. ) ;
#375 = EDGE_CURVE ( 'NONE', #12413, #5462, #9445, .T. ) ;
#376 = AXIS2_PLACEMENT_3D ( 'NONE', #11944, #14654, #7580 ) ;
#377 = DIRECTION ( 'NONE',  ( -1.000000000000000000, 0.000000000000000000, 4.336808689942021680E-16 ) ) ;
#378 = CIRCLE ( 'NONE', #5105, 0.9999999999999991118 ) ;
#379 = EDGE_CURVE ( 'NONE', #12310, #9517, #6444, .T. ) ;
#380 = CARTESIAN_POINT ( 'NONE',  ( 3.518350579753631191, 31.87180007765647716, 1.080741659609802285 ) ) ;
#381 = CARTESIAN_POINT ( 'NONE',  ( 9.178358240570380744, -10.00000000000000000, -2.937375903338058869 ) ) ;
#382 = ADVANCED_FACE ( 'NONE', ( #6168 ), #798, .T. ) ;
#383 = CARTESIAN_POINT ( 'NONE',  ( -4.243569643750004339, -23.78856235711027267, -5.420617734505230878 ) ) ;
#384 = CARTESIAN_POINT ( 'NONE',  ( 1.444289557196047680, 32.24680007765647360, 4.262301884875704161 ) ) ;
#385 = ADVANCED_FACE ( 'NONE', ( #4681 ), #10332, .T. ) ;
#386 = FACE_OUTER_BOUND ( 'NONE', #16135, .T. ) ;
#387 = ORIENTED_EDGE ( 'NONE', *, *, #14732, .T. ) ;
#388 = CARTESIAN_POINT ( 'NONE',  ( 3.500000000000000444, 31.74680007765647716, -0.05647727720536935281 ) ) ;
#389 = DIRECTION ( 'NONE',  ( 0.000000000000000000, 0.000000000000000000, 1.000000000000000000 ) ) ;
#390 = PLANE ( 'NONE',  #7793 ) ;
#391 = AXIS2_PLACEMENT_3D ( 'NONE', #10919, #2589, #8131 ) ;
#392 = DIRECTION ( 'NONE',  ( 0.000000000000000000, -1.000000000000000000, 0.000000000000000000 ) ) ;
#393 = ORIENTED_EDGE ( 'NONE', *, *, #5115, .F. ) ;
#394 = PRESENTATION_LAYER_ASSIGNMENT (  '', '', ( #2765 ) ) ;
#395 = CARTESIAN_POINT ( 'NONE',  ( -2.211161402132839182, 26.62819992234353705, 2.942372952327218627 ) ) ;
#396 = CARTESIAN_POINT ( 'NONE',  ( 0.000000000000000000, 33.00000000000000000, 0.000000000000000000 ) ) ;
#397 = CARTESIAN_POINT ( 'NONE',  ( -2.121784821875005722, -23.99619698609053842, -3.581405660193354379 ) ) ;
#398 = CARTESIAN_POINT ( 'NONE',  ( 3.481649420246369697, 36.62180007765648071, -1.193696214020541824 ) ) ;
#399 = CARTESIAN_POINT ( 'NONE',  ( 3.518350579753605434, 33.12819992234354771, -1.080741659609877114 ) ) ;
#400 = CARTESIAN_POINT ( 'NONE',  ( 1.999999999999994449, -22.66729209833581749, -2.051291100440815640 ) ) ;
#401 = CARTESIAN_POINT ( 'NONE',  ( 0.000000000000000000, 43.00000000000000000, -6.499999999999999112 ) ) ;
#402 = CARTESIAN_POINT ( 'NONE',  ( 4.730628863548789710E-15, -18.91846847603547133, -11.27987320052540809 ) ) ;
#403 = DIRECTION ( 'NONE',  ( -1.000000000000000000, 0.000000000000000000, 0.000000000000000000 ) ) ;
#404 = CIRCLE ( 'NONE', #10754, 2.000000000000000444 ) ;
#405 = VECTOR ( 'NONE', #13165, 1000.000000000000000 ) ;
#406 = DIRECTION ( 'NONE',  ( -0.000000000000000000, -1.000000000000000000, -0.000000000000000000 ) ) ;
#407 = FACE_OUTER_BOUND ( 'NONE', #5763, .T. ) ;
#408 = FACE_OUTER_BOUND ( 'NONE', #14459, .T. ) ;
#409 = ORIENTED_EDGE ( 'NONE', *, *, #7785, .F. ) ;
#410 = ORIENTED_EDGE ( 'NONE', *, *, #11507, .T. ) ;
#411 = LINE ( 'NONE', #3377, #16857 ) ;
#412 = CARTESIAN_POINT ( 'NONE',  ( -6.938893903907228378E-15, 6.938893903907228378E-15, 30.00000000000000000 ) ) ;
#413 =( NAMED_UNIT ( * ) SI_UNIT ( $, .STERADIAN. ) SOLID_ANGLE_UNIT ( ) );
#414 = ORIENTED_EDGE ( 'NONE', *, *, #4650, .T. ) ;
#415 = CARTESIAN_POINT ( 'NONE',  ( -0.05938372350921170689, 23.87819992234354416, 2.628655560595669183 ) ) ;
#416 = CARTESIAN_POINT ( 'NONE',  ( -2.121784821874996396, -22.44926158312459208, -14.18662328281289398 ) ) ;
#417 = CARTESIAN_POINT ( 'NONE',  ( 3.481649420246369697, 16.62180007765648071, -1.193696214020541824 ) ) ;
#418 = VECTOR ( 'NONE', #12172, 1000.000000000000000 ) ;
#419 = DIRECTION ( 'NONE',  ( -0.000000000000000000, -0.5735764363510414965, -0.8191520442889950182 ) ) ;
#420 = DIRECTION ( 'NONE',  ( -0.000000000000000000, -1.000000000000000000, -0.000000000000000000 ) ) ;
#421 = ORIENTED_EDGE ( 'NONE', *, *, #3365, .T. ) ;
#422 = CARTESIAN_POINT ( 'NONE',  ( 1.027846397803542144, 38.74680007765647360, -3.346150245485522312 ) ) ;
#423 = CARTESIAN_POINT ( 'NONE',  ( -2.121784821874996396, -24.03018163581715072, -16.44441110488443769 ) ) ;
#424 = DIRECTION ( 'NONE',  ( 1.027440012549754468E-14, -0.1129545544106655003, 0.9936001553129347741 ) ) ;
#425 = CARTESIAN_POINT ( 'NONE',  ( -4.243569643750004339, -27.66020330247980041, -10.94989403345594425 ) ) ;
#426 = DIRECTION ( 'NONE',  ( -0.000000000000000000, -1.000000000000000000, -0.000000000000000000 ) ) ;
#427 = LINE ( 'NONE', #3021, #14208 ) ;
#428 = CARTESIAN_POINT ( 'NONE',  ( 4.730628863548789710E-15, -20.95107997235447073, -14.18274325747453268 ) ) ;
#429 = DIRECTION ( 'NONE',  ( 0.000000000000000000, 0.000000000000000000, 1.000000000000000000 ) ) ;
#430 = CARTESIAN_POINT ( 'NONE',  ( -2.000000000000005773, -23.74274791649401095, -3.587201183482685352 ) ) ;
#431 = CARTESIAN_POINT ( 'NONE',  ( -1.593127413382998459, 25.87180007765647716, -2.091722143975139669 ) ) ;
#432 = ORIENTED_EDGE ( 'NONE', *, *, #4382, .T. ) ;
#433 = CARTESIAN_POINT ( 'NONE',  ( 2.211161402132902243, 24.62180007765647716, 2.942372952327172442 ) ) ;
#434 = CARTESIAN_POINT ( 'NONE',  ( -1.661723472263481630E-14, -21.09148155414254688, -12.81406445585025544 ) ) ;
#435 = CARTESIAN_POINT ( 'NONE',  ( -1.999999999999996225, -22.79950167706030228, -14.31905966800409402 ) ) ;
#436 = CARTESIAN_POINT ( 'NONE',  ( 14.99999999999999822, 13.00000000000000178, -25.00000000000000355 ) ) ;
#437 = CARTESIAN_POINT ( 'NONE',  ( -1.027846397803611866, 22.50319992234354416, -3.346150245485499219 ) ) ;
#438 =( BOUNDED_CURVE ( )  B_SPLINE_CURVE ( 2, ( #16331, #7967, #17558, #7596, #9268, #13622, #17653, #13255, #13442 ),
 .UNSPECIFIED., .F., .T. ) 
 B_SPLINE_CURVE_WITH_KNOTS ( ( 3, 2, 2, 2, 3 ),
 ( 0.5603448275862069616, 0.5632183908045976795, 0.5689655172413793371, 0.5747126436781608838, 0.5775862068965517127 ),
 .UNSPECIFIED. ) 
 CURVE ( )  GEOMETRIC_REPRESENTATION_ITEM ( )  RATIONAL_B_SPLINE_CURVE ( ( 0.9330127018922194093, 0.9330127018922206306, 1.000000000000000000, 0.8660254037844387076, 1.000000000000000000, 0.8660254037844387076, 1.000000000000000000, 0.9330127018922194093, 0.9330127018922194093 ) ) 
 REPRESENTATION_ITEM ( '' )  );
#439 = ORIENTED_EDGE ( 'NONE', *, *, #5539, .T. ) ;
#440 = CARTESIAN_POINT ( 'NONE',  ( -4.243569643750000786, -24.15837584640520674, -10.22025624374954766 ) ) ;
#441 = CARTESIAN_POINT ( 'NONE',  ( -3.518350579753630747, 18.12180007765648071, -1.080741659609802729 ) ) ;
#442 = ORIENTED_EDGE ( 'NONE', *, *, #6706, .F. ) ;
#443 =( LENGTH_UNIT ( ) NAMED_UNIT ( * ) SI_UNIT ( .MILLI., .METRE. ) );
#444 = EDGE_CURVE ( 'NONE', #6995, #13000, #16882, .T. ) ;
#445 = DIRECTION ( 'NONE',  ( -0.000000000000000000, 0.000000000000000000, -1.000000000000000000 ) ) ;
#446 = CARTESIAN_POINT ( 'NONE',  ( -2.121784821875005722, -29.19064858779466221, -10.99985136128556462 ) ) ;
#447 = CARTESIAN_POINT ( 'NONE',  ( -1.071796769724491671, -22.11239243885559347, -14.27207630091453261 ) ) ;
#448 = DIRECTION ( 'NONE',  ( -0.000000000000000000, -0.5735764363510414965, -0.8191520442889950182 ) ) ;
#449 = CARTESIAN_POINT ( 'NONE',  ( 2.000000000000004441, -19.68067980369657377, -9.864920426175917356 ) ) ;
#450 = CARTESIAN_POINT ( 'NONE',  ( 2.121784821874994176, -24.75977061698287329, -4.671901819153075230 ) ) ;
#451 = VERTEX_POINT ( 'NONE', #17514 ) ;
#452 = DIRECTION ( 'NONE',  ( -0.000000000000000000, -0.000000000000000000, 1.000000000000000000 ) ) ;
#453 = CARTESIAN_POINT ( 'NONE',  ( 1.071796769724485232, -25.63282338525647575, -5.352198374921374402 ) ) ;
#454 = DIRECTION ( 'NONE',  ( 3.469446951953612217E-16, -0.000000000000000000, 1.000000000000000000 ) ) ;
#455 = ORIENTED_EDGE ( 'NONE', *, *, #6941, .T. ) ;
#456 = VERTEX_POINT ( 'NONE', #14988 ) ;
#457 = DIRECTION ( 'NONE',  ( 0.000000000000000000, 0.8191520442889952403, -0.5735764363510413855 ) ) ;
#458 = DIRECTION ( 'NONE',  ( 0.000000000000000000, 0.8191520442889952403, -0.5735764363510413855 ) ) ;
#459 =( NAMED_UNIT ( * ) PLANE_ANGLE_UNIT ( ) SI_UNIT ( $, .RADIAN. ) );
#460 = CARTESIAN_POINT ( 'NONE',  ( -0.05938372350918959958, 28.87819992234354416, 4.731580009072201776 ) ) ;
#461 = CARTESIAN_POINT ( 'NONE',  ( -2.115076519116425580, 24.87819992234354416, -3.012182706137063182 ) ) ;
#462 = CARTESIAN_POINT ( 'NONE',  ( -2.500000000000001332, 22.00319992234354771, -0.05647727720530596601 ) ) ;
#463 = ORIENTED_EDGE ( 'NONE', *, *, #2191, .T. ) ;
#464 = CARTESIAN_POINT ( 'NONE',  ( -4.481649420246366589, 17.87180007765647360, 1.518615910253458878 ) ) ;
#465 = CARTESIAN_POINT ( 'NONE',  ( -5.279047395330986450E-15, -26.40935253139716110, -5.382348295486703016 ) ) ;
#466 = ORIENTED_EDGE ( 'NONE', *, *, #14601, .T. ) ;
#467 = LINE ( 'NONE', #4822, #15982 ) ;
#468 = CARTESIAN_POINT ( 'NONE',  ( 2.798362969681366330, 26.49680007765648071, -2.102939460078824929 ) ) ;
#469 = DIRECTION ( 'NONE',  ( -4.915049848600951133E-16, 0.000000000000000000, -1.000000000000000000 ) ) ;
#470 = CARTESIAN_POINT ( 'NONE',  ( -4.243569643750000786, -21.28690881192279960, -6.119376322027766157 ) ) ;
#471 = CARTESIAN_POINT ( 'NONE',  ( -1.336863392178478716, 32.49680007765647360, 4.297206761780677731 ) ) ;
#472 = CARTESIAN_POINT ( 'NONE',  ( 1.071796769724495224, -16.65062116698148031, -6.471858545706086652 ) ) ;
#473 = ORIENTED_EDGE ( 'NONE', *, *, #4672, .F. ) ;
#474 = AXIS2_PLACEMENT_3D ( 'NONE', #12018, #10254, #3231 ) ;
#475 = CARTESIAN_POINT ( 'NONE',  ( 2.115076519116362963, 28.87180007765647716, -3.012182706137107147 ) ) ;
#476 = CARTESIAN_POINT ( 'NONE',  ( 4.253155871621279616, -10.96494312749350186, 19.45022984308079472 ) ) ;
#477 = EDGE_CURVE ( 'NONE', #6613, #1681, #7918, .T. ) ;
#478 = DIRECTION ( 'NONE',  ( -0.000000000000000000, -0.5735764363510414965, -0.8191520442889950182 ) ) ;
#479 = CARTESIAN_POINT ( 'NONE',  ( 4.898587196589417759E-16, -3.999999999999993339, 25.54267522293723758 ) ) ;
#480 =( NAMED_UNIT ( * ) PLANE_ANGLE_UNIT ( ) SI_UNIT ( $, .RADIAN. ) );
#481 = ORIENTED_EDGE ( 'NONE', *, *, #17047, .T. ) ;
#482 = CARTESIAN_POINT ( 'NONE',  ( 0.05938372350920109732, 30.12819992234354416, -3.680117784833935701 ) ) ;
#483 = EDGE_CURVE ( 'NONE', #4093, #15831, #6358, .T. ) ;
#484 = DIRECTION ( 'NONE',  ( 0.000000000000000000, 0.000000000000000000, -1.000000000000000000 ) ) ;
#485 = CARTESIAN_POINT ( 'NONE',  ( 4.730628863548789710E-15, -16.82132963062697684, -8.284848538593767131 ) ) ;
#486 = CARTESIAN_POINT ( 'NONE',  ( 1.497042530366477164, 18.87180007765648071, -2.161531897785062384 ) ) ;
#487 = CARTESIAN_POINT ( 'NONE',  ( 3.673772985318163098, 18.00319992234354416, -2.599342558261029001 ) ) ;
#488 = CARTESIAN_POINT ( 'NONE',  ( 4.243569643749997233, -28.89697749336173871, -12.71619062895408803 ) ) ;
#489 = CARTESIAN_POINT ( 'NONE',  ( -4.000000000000004441, -28.17415170002511360, -11.92906061754144886 ) ) ;
#490 = AXIS2_PLACEMENT_3D ( 'NONE', #9577, #2373, #2640 ) ;
#491 = ADVANCED_FACE ( 'NONE', ( #892 ), #2289, .F. ) ;
#492 = CARTESIAN_POINT ( 'NONE',  ( -4.243569643750000786, -21.83539127918348299, -6.902690464379118040 ) ) ;
#493 = AXIS2_PLACEMENT_3D ( 'NONE', #9507, #8120, #16856 ) ;
#494 = CARTESIAN_POINT ( 'NONE',  ( 0.000000000000000000, 33.00000000000000000, 0.000000000000000000 ) ) ;
#495 = CARTESIAN_POINT ( 'NONE',  ( -0.3267727178421339085, -10.00000000000000178, -5.052762561669631225 ) ) ;
#496 = FACE_OUTER_BOUND ( 'NONE', #17631, .T. ) ;
#497 = FACE_OUTER_BOUND ( 'NONE', #16040, .T. ) ;
#498 = ORIENTED_EDGE ( 'NONE', *, *, #5184, .F. ) ;
#499 = ORIENTED_EDGE ( 'NONE', *, *, #6216, .T. ) ;
#500 = CARTESIAN_POINT ( 'NONE',  ( 2.121784821874994176, -22.92074116793234140, -2.045495577151484223 ) ) ;
#501 = CARTESIAN_POINT ( 'NONE',  ( -6.428571428571423496, -11.73421655796351892, 14.25837509840161310 ) ) ;
#502 = DIRECTION ( 'NONE',  ( -0.000000000000000000, 1.000000000000000000, -0.000000000000000000 ) ) ;
#503 = ORIENTED_EDGE ( 'NONE', *, *, #11462, .F. ) ;
#504 = CARTESIAN_POINT ( 'NONE',  ( -2.518350579753611207, 26.87819992234354416, 0.7558219633769609480 ) ) ;
#505 =( NAMED_UNIT ( * ) SI_UNIT ( $, .STERADIAN. ) SOLID_ANGLE_UNIT ( ) );
#506 = EDGE_CURVE ( 'NONE', #17004, #8682, #13300, .T. ) ;
#507 = CIRCLE ( 'NONE', #12335, 4.000000000000000000 ) ;
#508 = CARTESIAN_POINT ( 'NONE',  ( -4.243569643750000786, -26.19098734272420614, -13.12312630069867225 ) ) ;
#509 = CARTESIAN_POINT ( 'NONE',  ( -2.798362969681365886, 20.24680007765647716, 2.102939460078824929 ) ) ;
#510 = DIRECTION ( 'NONE',  ( -1.000000000000000000, -0.000000000000000000, -0.000000000000000000 ) ) ;
#511 = CARTESIAN_POINT ( 'NONE',  ( 4.757769075324610242, -14.90261145393154862, -7.125238870422657911 ) ) ;
#512 = ORIENTED_EDGE ( 'NONE', *, *, #13369, .F. ) ;
#513 = FACE_OUTER_BOUND ( 'NONE', #11617, .T. ) ;
#514 = CARTESIAN_POINT ( 'NONE',  ( 2.121784821875004390, -23.29887167946958115, -15.39999224841596437 ) ) ;
#515 = SURFACE_STYLE_FILL_AREA ( #13112 ) ;
#516 = CIRCLE ( 'NONE', #8483, 4.400000000000002132 ) ;
#517 = CARTESIAN_POINT ( 'NONE',  ( 2.121784821875004390, -21.20173283406107956, -12.40496758648432518 ) ) ;
#518 = CARTESIAN_POINT ( 'NONE',  ( -8.500000000000007105, 14.80000000000000071, -20.49999999999999645 ) ) ;
#519 = CARTESIAN_POINT ( 'NONE',  ( -1.071796769724486786, -16.95020451169621722, -6.899707902313577002 ) ) ;
#520 = EDGE_CURVE ( 'NONE', #156, #17729, #13398, .T. ) ;
#521 = LINE ( 'NONE', #2012, #6452 ) ;
#522 = CARTESIAN_POINT ( 'NONE',  ( -5.330712181944245322E-15, -27.81736316408238707, -6.902851464902143519 ) ) ;
#523 = CARTESIAN_POINT ( 'NONE',  ( -5.577813053751546416E-15, -25.96698683212770931, -5.829433235496615850 ) ) ;
#524 = DIRECTION ( 'NONE',  ( 0.000000000000000000, 0.000000000000000000, -1.000000000000000000 ) ) ;
#525 = CARTESIAN_POINT ( 'NONE',  ( 1.497042530366477164, 33.87180007765647360, -2.161531897785062384 ) ) ;
#526 = VERTEX_POINT ( 'NONE', #13484 ) ;
#527 = CARTESIAN_POINT ( 'NONE',  ( -2.115076519116362519, 25.12180007765647005, 3.012182706137108035 ) ) ;
#528 = CARTESIAN_POINT ( 'NONE',  ( -8.500000000000010658, 17.19999999999999929, 20.49999999999998934 ) ) ;
#529 = CARTESIAN_POINT ( 'NONE',  ( 2.000000000000004441, -22.58441051342866857, -14.01187765139572150 ) ) ;
#530 = CARTESIAN_POINT ( 'NONE',  ( 1.071796769724504328, -23.63247556418714979, -2.495405621470275559 ) ) ;
#531 = CIRCLE ( 'NONE', #12662, 1.250000000000000222 ) ;
#532 = CARTESIAN_POINT ( 'NONE',  ( 1.027846397803612311, 18.75319992234354771, 3.346150245485499219 ) ) ;
#533 = ORIENTED_EDGE ( 'NONE', *, *, #16187, .T. ) ;
#534 = CARTESIAN_POINT ( 'NONE',  ( 4.243569643750000786, -22.99688356279435197, -8.561473354064329300 ) ) ;
#535 = CARTESIAN_POINT ( 'NONE',  ( -2.864755990943265829, 18.24680007765648071, -2.011557305968488141 ) ) ;
#536 = ORIENTED_EDGE ( 'NONE', *, *, #1348, .T. ) ;
#537 =( NAMED_UNIT ( * ) PLANE_ANGLE_UNIT ( ) SI_UNIT ( $, .RADIAN. ) );
#538 = DIRECTION ( 'NONE',  ( -1.000000000000000000, 0.000000000000000000, 0.000000000000000000 ) ) ;
#539 = CLOSED_SHELL ( 'NONE', ( #14555, #17882, #8237, #2719, #9820 ) ) ;
#540 = CARTESIAN_POINT ( 'NONE',  ( -4.243569643749997233, -23.97970686843945742, -14.23658061064251257 ) ) ;
#541 = CARTESIAN_POINT ( 'NONE',  ( 1.999999999999994449, -29.57171845020653222, -11.91183383256282724 ) ) ;
#542 = DIRECTION ( 'NONE',  ( -1.000000000000000000, -0.000000000000000000, -0.000000000000000000 ) ) ;
#544 = CARTESIAN_POINT ( 'NONE',  ( -1.071796769724486564, -28.23697075027383008, -9.071306243533678426 ) ) ;
#543 = AXIS2_PLACEMENT_3D ( 'NONE', #16285, #14984, #3573 ) ;
#545 = CARTESIAN_POINT ( 'NONE',  ( 4.243569643750000786, -20.15768020285669593, -4.506670734833804204 ) ) ;
#546 = ORIENTED_EDGE ( 'NONE', *, *, #16871, .T. ) ;
#547 = CARTESIAN_POINT ( 'NONE',  ( -4.000000000000000888, -23.52923419313512454, -9.321748845673438311 ) ) ;
#548 = EDGE_CURVE ( 'NONE', #8360, #17559, #7326, .T. ) ;
#549 = CARTESIAN_POINT ( 'NONE',  ( 4.000000000000000888, -22.88396070224021273, -8.400202795848317194 ) ) ;
#550 = DIRECTION ( 'NONE',  ( 0.000000000000000000, 0.000000000000000000, 1.000000000000000000 ) ) ;
#551 = ORIENTED_EDGE ( 'NONE', *, *, #7099, .T. ) ;
#552 = EDGE_LOOP ( 'NONE', ( #5619, #2064, #7284, #8498 ) ) ;
#553 =( BOUNDED_CURVE ( )  B_SPLINE_CURVE ( 2, ( #11093, #6833, #15203, #6742, #11181, #13792, #1101, #18087, #9699 ),
 .UNSPECIFIED., .F., .T. ) 
 B_SPLINE_CURVE_WITH_KNOTS ( ( 3, 2, 2, 2, 3 ),
 ( 0.9051724137931034253, 0.9080459770114942541, 0.9137931034482759118, 0.9195402298850574585, 0.9224137931034482873 ),
 .UNSPECIFIED. ) 
 CURVE ( )  GEOMETRIC_REPRESENTATION_ITEM ( )  RATIONAL_B_SPLINE_CURVE ( ( 0.9330127018922194093, 0.9330127018922194093, 1.000000000000000000, 0.8660254037844387076, 1.000000000000000000, 0.8660254037844387076, 1.000000000000000000, 0.9330127018922194093, 0.9330127018922194093 ) ) 
 REPRESENTATION_ITEM ( '' )  );
#554 = CARTESIAN_POINT ( 'NONE',  ( -8.500000000000007105, 15.00000000000000000, -20.49999999999999645 ) ) ;
#555 = ADVANCED_FACE ( 'NONE', ( #15075 ), #3750, .F. ) ;
#556 = DIRECTION ( 'NONE',  ( 0.000000000000000000, 0.8191520442889952403, -0.5735764363510413855 ) ) ;
#557 =( NAMED_UNIT ( * ) SI_UNIT ( $, .STERADIAN. ) SOLID_ANGLE_UNIT ( ) );
#558 = CARTESIAN_POINT ( 'NONE',  ( 4.499999999999999112, 23.25319992234354416, 0.05647727720528474687 ) ) ;
#559 = CARTESIAN_POINT ( 'NONE',  ( -2.115076519116425580, 37.37819992234353350, -3.012182706137063182 ) ) ;
#560 = EDGE_CURVE ( 'NONE', #14256, #10497, #11069, .T. ) ;
#561 = CARTESIAN_POINT ( 'NONE',  ( -2.481649420246391902, 19.62819992234354416, -0.8687765177875723666 ) ) ;
#562 = ORIENTED_EDGE ( 'NONE', *, *, #12720, .F. ) ;
#563=STYLED_ITEM('',(#18424),#14467);
#564 = CARTESIAN_POINT ( 'NONE',  ( 3.673772985318219053, 19.49680007765647005, 2.599342558260951730 ) ) ;
#565 = CIRCLE ( 'NONE', #15638, 8.000000000000001776 ) ;
#566 = CARTESIAN_POINT ( 'NONE',  ( 4.713407268011036227E-15, -18.97140477713641005, -10.86512966430133176 ) ) ;
#567 = ORIENTED_EDGE ( 'NONE', *, *, #8137, .F. ) ;
#568 = DIRECTION ( 'NONE',  ( 0.000000000000000000, -1.000000000000000000, 0.000000000000000000 ) ) ;
#569 = CARTESIAN_POINT ( 'NONE',  ( -3.481649420246369697, 32.87180007765645939, 1.193696214020542490 ) ) ;
#570 = CARTESIAN_POINT ( 'NONE',  ( 1.071796769724485454, -20.52226211235100806, -12.00113484465680358 ) ) ;
#571 = CARTESIAN_POINT ( 'NONE',  ( -4.243569643749998122, -19.55958345580924629, -7.923990169340444645 ) ) ;
#572 = CARTESIAN_POINT ( 'NONE',  ( 4.518350579753633411, 29.37180007765647716, 1.405661355842698468 ) ) ;
#573 = AXIS2_PLACEMENT_3D ( 'NONE', #13525, #13619, #11017 ) ;
#574 = CARTESIAN_POINT ( 'NONE',  ( 3.999999999999996447, -28.41075198072487140, -12.26696083681741989 ) ) ;
#575 = CIRCLE ( 'NONE', #9148, 0.4000000000000001887 ) ;
#576 = ORIENTED_EDGE ( 'NONE', *, *, #8996, .F. ) ;
#577 = CARTESIAN_POINT ( 'NONE',  ( 2.531783071939769592, -10.67720498481739355, 21.39218517664858510 ) ) ;
#578 = CARTESIAN_POINT ( 'NONE',  ( 0.000000000000000000, 5.977523610840987267, 32.81826849749789687 ) ) ;
#579 = DIRECTION ( 'NONE',  ( -3.469446951953613696E-16, -0.000000000000000000, -1.000000000000000000 ) ) ;
#580 = FILL_AREA_STYLE_COLOUR ( '', #14162 ) ;
#581 = ORIENTED_EDGE ( 'NONE', *, *, #2191, .F. ) ;
#582 = CARTESIAN_POINT ( 'NONE',  ( -3.500000000000000444, 24.50319992234354416, -0.05647727720529563400 ) ) ;
#583 = LINE ( 'NONE', #2071, #18170 ) ;
#584 = CARTESIAN_POINT ( 'NONE',  ( 4.243569643749996345, -23.18630709894168263, -4.560508088001781424 ) ) ;
#585 = CARTESIAN_POINT ( 'NONE',  ( 2.500000000000001332, 24.24680007765647716, -0.05647727720535888202 ) ) ;
#586 = CARTESIAN_POINT ( 'NONE',  ( -3.673772985318163098, 16.75319992234354416, 2.599342558261029001 ) ) ;
#587 = CARTESIAN_POINT ( 'NONE',  ( 4.243569643749997233, -28.38075870064580286, -11.97895378909399078 ) ) ;
#588 = CARTESIAN_POINT ( 'NONE',  ( 1.999999999999994449, -29.31360905384856608, -11.54321541263277950 ) ) ;
#589 = VECTOR ( 'NONE', #2601, 1000.000000000000000 ) ;
#590 = CARTESIAN_POINT ( 'NONE',  ( 2.121784821875004390, -18.13668375231020846, -8.027623849815011425 ) ) ;
#591 = LINE ( 'NONE', #14501, #12766 ) ;
#592 = EDGE_CURVE ( 'NONE', #196, #11177, #4131, .T. ) ;
#593 = DIRECTION ( 'NONE',  ( 1.000000000000000000, 0.000000000000000000, 1.224646799147353207E-16 ) ) ;
#594 = DIRECTION ( 'NONE',  ( 0.000000000000000000, 0.000000000000000000, -1.000000000000000000 ) ) ;
#595 = ORIENTED_EDGE ( 'NONE', *, *, #1110, .F. ) ;
#596 = ORIENTED_EDGE ( 'NONE', *, *, #6615, .F. ) ;
#597 = FILL_AREA_STYLE_COLOUR ( '', #8522 ) ;
#598 = CARTESIAN_POINT ( 'NONE',  ( 4.299564228933482956E-15, -17.41342265533655009, -7.561251970840314307 ) ) ;
#599 = CARTESIAN_POINT ( 'NONE',  ( -31.74999999999995737, 0.000000000000000000, 0.000000000000000000 ) ) ;
#600 = ORIENTED_EDGE ( 'NONE', *, *, #8861, .F. ) ;
#601 = CIRCLE ( 'NONE', #17798, 0.9999999999999991118 ) ;
#602 = CARTESIAN_POINT ( 'NONE',  ( -1.497042530366522461, 27.37819992234355126, -2.161531897785030409 ) ) ;
#603 =( NAMED_UNIT ( * ) PLANE_ANGLE_UNIT ( ) SI_UNIT ( $, .RADIAN. ) );
#604 = CARTESIAN_POINT ( 'NONE',  ( 4.730628863548789710E-15, -22.24162695414431212, -16.02583535712476959 ) ) ;
#605 = CARTESIAN_POINT ( 'NONE',  ( 0.05938372350927906274, 24.87180007765647005, 3.680117784833935701 ) ) ;
#606 = DIRECTION ( 'NONE',  ( 0.000000000000000000, 0.000000000000000000, -1.000000000000000000 ) ) ;
#607 = CARTESIAN_POINT ( 'NONE',  ( 2.121784821875004390, -22.00832469767973620, -13.55690014876572569 ) ) ;
#608 = AXIS2_PLACEMENT_3D ( 'NONE', #7534, #13468, #14602 ) ;
#609 = EDGE_CURVE ( 'NONE', #1376, #8485, #13946, .T. ) ;
#610 = VECTOR ( 'NONE', #3816, 1000.000000000000227 ) ;
#611 = CARTESIAN_POINT ( 'NONE',  ( 4.299564228933482956E-15, -21.02695420434810814, -12.72190984986098172 ) ) ;
#612 = EDGE_CURVE ( 'NONE', #11658, #10194, #17872, .T. ) ;
#613 = CARTESIAN_POINT ( 'NONE',  ( 2.121784821874994176, -27.05049150965984595, -7.943390296032248443 ) ) ;
#614 = FACE_OUTER_BOUND ( 'NONE', #3164, .T. ) ;
#615 = ADVANCED_FACE ( 'NONE', ( #13762 ), #4118, .F. ) ;
#616 = CARTESIAN_POINT ( 'NONE',  ( -1.734723475976807094E-15, 31.99999999999999289, -2.500000000000000000 ) ) ;
#617 = CARTESIAN_POINT ( 'NONE',  ( -31.74999999999995737, 0.000000000000000000, 0.000000000000000000 ) ) ;
#618 = CARTESIAN_POINT ( 'NONE',  ( 4.243569643749996345, -25.25118226980542602, -7.509455447442161535 ) ) ;
#619 = ORIENTED_EDGE ( 'NONE', *, *, #1520, .F. ) ;
#620 = CYLINDRICAL_SURFACE ( 'NONE', #17533, 4.000000000000000000 ) ;
#621 = CARTESIAN_POINT ( 'NONE',  ( 2.610817454768295409, -22.11373505648317916, -1.875566028523329098 ) ) ;
#622 = CARTESIAN_POINT ( 'NONE',  ( -2.518350579753628526, 28.12180007765647716, -0.7558219633769075463 ) ) ;
#623 = ORIENTED_EDGE ( 'NONE', *, *, #10806, .F. ) ;
#624 = CARTESIAN_POINT ( 'NONE',  ( 2.211161402132902243, 27.12180007765647716, 2.942372952327172442 ) ) ;
#625 = DIRECTION ( 'NONE',  ( -0.000000000000000000, -0.5735764363510414965, -0.8191520442889950182 ) ) ;
#626 = SHAPE_DEFINITION_REPRESENTATION ( #10627, #8990 ) ;
#627 = AXIS2_PLACEMENT_3D ( 'NONE', #9610, #15282, #8214 ) ;
#628 = LINE ( 'NONE', #9232, #14321 ) ;
#629 = CARTESIAN_POINT ( 'NONE',  ( 3.481649420246394122, 20.87819992234354416, 1.193696214020467439 ) ) ;
#630 = APPLICATION_CONTEXT ( 'automotive_design' ) ;
#631 = EDGE_LOOP ( 'NONE', ( #5395, #16207, #13707, #2530 ) ) ;
#632 = CARTESIAN_POINT ( 'NONE',  ( 4.243569643750000786, -22.48066477007841613, -7.824236514204232940 ) ) ;
#633 = CARTESIAN_POINT ( 'NONE',  ( 3.500000000000000444, 16.74680007765647716, -0.05647727720536935281 ) ) ;
#634 = VERTEX_POINT ( 'NONE', #16468 ) ;
#635 = SURFACE_STYLE_FILL_AREA ( #2123 ) ;
#636 = FACE_OUTER_BOUND ( 'NONE', #10821, .T. ) ;
#637 = CARTESIAN_POINT ( 'NONE',  ( -4.243569643750005227, -26.91813878795063886, -9.890116076157061897 ) ) ;
#638 = CARTESIAN_POINT ( 'NONE',  ( -6.158835246850665095E-15, -22.12391913957442213, -14.28853813557044639 ) ) ;
#639 = B_SPLINE_CURVE_WITH_KNOTS ( 'NONE', 1,
 ( #5800, #5891 ),
 .UNSPECIFIED., .F., .F.,
 ( 2, 2 ),
 ( 0.000000000000000000, 1.000000000000000000 ),
 .UNSPECIFIED. ) ;
#640 = AXIS2_PLACEMENT_3D ( 'NONE', #16166, #307, #1699 ) ;
#641 = CARTESIAN_POINT ( 'NONE',  ( 7.381087143211832569, -10.35722647083040826, 4.976872143527621084 ) ) ;
#642 = CARTESIAN_POINT ( 'NONE',  ( -4.243569643750000786, -26.96531553179811169, -14.22898156048881724 ) ) ;
#643 = ORIENTED_EDGE ( 'NONE', *, *, #13613, .T. ) ;
#644 = DIRECTION ( 'NONE',  ( -4.915049848600951133E-16, 0.000000000000000000, -1.000000000000000000 ) ) ;
#645 = CARTESIAN_POINT ( 'NONE',  ( 1.999999999999994449, -26.02271425098940938, -6.843330559531437984 ) ) ;
#646 = VERTEX_POINT ( 'NONE', #1074 ) ;
#647 = ORIENTED_EDGE ( 'NONE', *, *, #2644, .T. ) ;
#648 = CARTESIAN_POINT ( 'NONE',  ( 10.00000000000000355, 27.59999999999999432, 2.499999999999996891 ) ) ;
#649 = CYLINDRICAL_SURFACE ( 'NONE', #8066, 4.000000000000000000 ) ;
#650 = CARTESIAN_POINT ( 'NONE',  ( -4.499999999999999112, 29.50319992234354061, -0.05647727720528529505 ) ) ;
#651 = CARTESIAN_POINT ( 'NONE',  ( -2.115076519116425580, 32.37819992234354771, -3.012182706137063182 ) ) ;
#652 = CARTESIAN_POINT ( 'NONE',  ( -0.05938372350921170689, 23.87819992234354416, 2.628655560595669183 ) ) ;
#653 = ORIENTED_EDGE ( 'NONE', *, *, #13216, .F. ) ;
#654 = AXIS2_PLACEMENT_3D ( 'NONE', #4844, #10493, #1896 ) ;
#655 = CARTESIAN_POINT ( 'NONE',  ( -1.444289557196047014, 15.99680007765647716, -4.262301884875704161 ) ) ;
#656 = CARTESIAN_POINT ( 'NONE',  ( -2.000000000000005773, -24.45254875577348130, -4.600901837283550400 ) ) ;
#657 = ORIENTED_EDGE ( 'NONE', *, *, #883, .F. ) ;
#658 = DIRECTION ( 'NONE',  ( 0.000000000000000000, 0.000000000000000000, 1.000000000000000000 ) ) ;
#659 = CARTESIAN_POINT ( 'NONE',  ( 3.518350579753631191, 36.87180007765645939, 1.080741659609802285 ) ) ;
#660 = EDGE_CURVE ( 'NONE', #8755, #15831, #10339, .T. ) ;
#661 = CARTESIAN_POINT ( 'NONE',  ( -2.121784821875005722, -23.22186879701663642, -2.475550400403212503 ) ) ;
#662 =( BOUNDED_CURVE ( )  B_SPLINE_CURVE ( 2, ( #13922, #1231, #6865, #12609, #13733, #12521, #9559, #14007, #12431 ),
 .UNSPECIFIED., .F., .F. ) 
 B_SPLINE_CURVE_WITH_KNOTS ( ( 3, 2, 2, 2, 3 ),
 ( 0.3534482758620690057, 0.3563218390804597790, 0.3620689655172413812, 0.3678160919540229834, 0.3706896551724138122 ),
 .UNSPECIFIED. ) 
 CURVE ( )  GEOMETRIC_REPRESENTATION_ITEM ( )  RATIONAL_B_SPLINE_CURVE ( ( 0.9330127018922194093, 0.9330127018922200755, 1.000000000000000000, 0.8660254037844387076, 1.000000000000000000, 0.8660254037844387076, 1.000000000000000000, 0.9330127018922187432, 0.9330127018922194093 ) ) 
 REPRESENTATION_ITEM ( '' )  );
#663 = CARTESIAN_POINT ( 'NONE',  ( 2.121784821874994176, -27.34086458056255964, -8.358086018453551702 ) ) ;
#664 = EDGE_CURVE ( 'NONE', #15831, #13916, #15675, .T. ) ;
#665 = CARTESIAN_POINT ( 'NONE',  ( 2.170367169212293224, -29.75460566901168491, -12.32900594437920816 ) ) ;
#666 = EDGE_LOOP ( 'NONE', ( #3881, #11701, #9259, #14886 ) ) ;
#667 = CARTESIAN_POINT ( 'NONE',  ( -4.772237607920192026, -11.09252097142725901, 18.58920227068528419 ) ) ;
#668 = CARTESIAN_POINT ( 'NONE',  ( 0.000000000000000000, 5.000000000000000000, 0.000000000000000000 ) ) ;
#669 = DIRECTION ( 'NONE',  ( -1.000000000000000000, 0.000000000000000000, 4.336808689942021680E-16 ) ) ;
#670 = CARTESIAN_POINT ( 'NONE',  ( 2.121784821875004390, -24.07319986854348670, -16.50584750820610580 ) ) ;
#671 = EDGE_LOOP ( 'NONE', ( #1237, #16466, #3525, #5028 ) ) ;
#672 = CARTESIAN_POINT ( 'NONE',  ( -1.027846397803611866, 30.00319992234354416, -3.346150245485499219 ) ) ;
#673 = CARTESIAN_POINT ( 'NONE',  ( 3.939448708636003271, -26.33660243321148897, -14.75747596281047436 ) ) ;
#674 = CARTESIAN_POINT ( 'NONE',  ( -5.330712181944245322E-15, -24.97815980414473103, -2.848048845671618423 ) ) ;
#675 = CARTESIAN_POINT ( 'NONE',  ( 2.481649420246374138, 19.12180007765648071, -0.8687765177876252132 ) ) ;
#676 = AXIS2_PLACEMENT_3D ( 'NONE', #7188, #2849, #8663 ) ;
#677 = CARTESIAN_POINT ( 'NONE',  ( -2.829195390882724315, 21.62819992234354416, 3.793023760679264722 ) ) ;
#678 = MECHANICAL_DESIGN_GEOMETRIC_PRESENTATION_REPRESENTATION (  '', ( #17571 ), #3617 ) ;
#679 = CARTESIAN_POINT ( 'NONE',  ( -4.243569643750000786, -26.99757920634285924, -14.27505886298007276 ) ) ;
#680 = CARTESIAN_POINT ( 'NONE',  ( -2.000000000000005773, -28.58229909750097875, -10.49879655616431506 ) ) ;
#681 =( GEOMETRIC_REPRESENTATION_CONTEXT ( 3 ) GLOBAL_UNCERTAINTY_ASSIGNED_CONTEXT ( ( #15795 ) ) GLOBAL_UNIT_ASSIGNED_CONTEXT ( ( #11823, #4782, #14341 ) ) REPRESENTATION_CONTEXT ( 'NONE', 'WORKASPACE' ) );
#682 = CARTESIAN_POINT ( 'NONE',  ( 4.243569643750000786, -21.96444597736247673, -7.086999674344137468 ) ) ;
#683 = CARTESIAN_POINT ( 'NONE',  ( -4.499999999999999112, 37.99680007765646650, 0.05647727720537927543 ) ) ;
#684 = EDGE_CURVE ( 'NONE', #10458, #6378, #13728, .T. ) ;
#685 = CYLINDRICAL_SURFACE ( 'NONE', #4943, 0.9999999999999991118 ) ;
#686 = AXIS2_PLACEMENT_3D ( 'NONE', #9405, #9497, #896 ) ;
#687 = CARTESIAN_POINT ( 'NONE',  ( 3.999999999999997780, -28.14205403674597861, -13.39922821167334810 ) ) ;
#688 =( GEOMETRIC_REPRESENTATION_CONTEXT ( 3 ) GLOBAL_UNCERTAINTY_ASSIGNED_CONTEXT ( ( #16960 ) ) GLOBAL_UNIT_ASSIGNED_CONTEXT ( ( #13427, #13926, #10357 ) ) REPRESENTATION_CONTEXT ( 'NONE', 'WORKASPACE' ) );
#689 = CARTESIAN_POINT ( 'NONE',  ( 1.999999999999994449, -25.50649545827347353, -6.106093719671341624 ) ) ;
#690 = ORIENTED_EDGE ( 'NONE', *, *, #8744, .T. ) ;
#691 = EDGE_LOOP ( 'NONE', ( #11697, #16402, #8918, #16963 ) ) ;
#692 = SURFACE_STYLE_USAGE ( .BOTH. , #7533 ) ;
#693 = CARTESIAN_POINT ( 'NONE',  ( 4.000000000000003553, -18.84129845210892640, -6.653000668470220980 ) ) ;
#694 = LINE ( 'NONE', #11983, #5859 ) ;
#695 = ORIENTED_EDGE ( 'NONE', *, *, #6775, .F. ) ;
#696 = CARTESIAN_POINT ( 'NONE',  ( 0.7188294034286553114, 26.25319992234354416, 2.395093729190349130 ) ) ;
#697 = CARTESIAN_POINT ( 'NONE',  ( 4.243569643750003451, -23.00104207391549593, -12.83890243507441120 ) ) ;
#698 = CARTESIAN_POINT ( 'NONE',  ( 1.135272562821090458, 19.74680007765648071, 3.311245368580554072 ) ) ;
#699 = DIRECTION ( 'NONE',  ( 1.000000000000000000, 0.000000000000000000, 0.000000000000000000 ) ) ;
#700 = CARTESIAN_POINT ( 'NONE',  ( -0.5181399714674771451, -9.999999999997587707, -3.173488174254735839 ) ) ;
#701 = CIRCLE ( 'NONE', #17888, 2.000000000000001776 ) ;
#702 = CARTESIAN_POINT ( 'NONE',  ( -4.243569643750000786, -25.19081343183707844, -11.69472992346973861 ) ) ;
#703 = CARTESIAN_POINT ( 'NONE',  ( 2.121784821874994176, -27.30860090601781209, -8.312008715962296179 ) ) ;
#704 = CARTESIAN_POINT ( 'NONE',  ( -6.938893903907228378E-15, 6.938893903907228378E-15, -4.999999999999997335 ) ) ;
#705 = CARTESIAN_POINT ( 'NONE',  ( -4.000000000000004441, -22.04405353722830085, -3.174373145209581804 ) ) ;
#706 = DIRECTION ( 'NONE',  ( 0.000000000000000000, -0.000000000000000000, -1.000000000000000000 ) ) ;
#707 = CARTESIAN_POINT ( 'NONE',  ( -2.121784821875005722, -26.31918155331226217, -6.898971439563784003 ) ) ;
#708 = ORIENTED_EDGE ( 'NONE', *, *, #8626, .T. ) ;
#709 = AXIS2_PLACEMENT_3D ( 'NONE', #11637, #13032, #6365 ) ;
#710 = CARTESIAN_POINT ( 'NONE',  ( -3.999999999999997335, -17.78735175101882859, -5.147808788095962207 ) ) ;
#711 = CARTESIAN_POINT ( 'NONE',  ( 1.497042530366477164, 28.87180007765648426, -2.161531897785062384 ) ) ;
#712 = EDGE_LOOP ( 'NONE', ( #2767, #16521, #3729, #8436, #3326, #6869 ) ) ;
#713 = CARTESIAN_POINT ( 'NONE',  ( 1.027846397803542144, 31.24680007765647716, -3.346150245485522312 ) ) ;
#714 = CARTESIAN_POINT ( 'NONE',  ( 4.000000000000000888, -23.91639828767208442, -9.874676475568506362 ) ) ;
#715 = ADVANCED_FACE ( 'NONE', ( #15445, #17962, #11152, #8375, #10887, #18056 ), #6533, .F. ) ;
#716 = SHAPE_DEFINITION_REPRESENTATION ( #7507, #1416 ) ;
#717 = CARTESIAN_POINT ( 'NONE',  ( 9.000000000000005329, -12.99999999999999822, -3.713574246709343996 ) ) ;
#718 = EDGE_CURVE ( 'NONE', #4345, #7195, #15626, .T. ) ;
#719 = ORIENTED_EDGE ( 'NONE', *, *, #15424, .F. ) ;
#720 = CARTESIAN_POINT ( 'NONE',  ( 2.121784821874994176, -25.53409880605677884, -5.777757078943218438 ) ) ;
#721 = ADVANCED_FACE ( 'NONE', ( #15892 ), #7066, .T. ) ;
#722 = CARTESIAN_POINT ( 'NONE',  ( -1.336863392178478716, 39.99680007765647360, 4.297206761780677731 ) ) ;
#723 = VERTEX_POINT ( 'NONE', #9855 ) ;
#724 = VECTOR ( 'NONE', #10694, 1000.000000000000000 ) ;
#725 = PRODUCT_DEFINITION_SHAPE ( 'NONE', 'NONE',  #2104 ) ;
#726 = EDGE_CURVE ( 'NONE', #17169, #13482, #4570, .T. ) ;
#727 = CARTESIAN_POINT ( 'NONE',  ( 3.999999999999996447, -23.44214610012902966, -5.171056252157234745 ) ) ;
#728 = DIRECTION ( 'NONE',  ( 0.000000000000000000, 0.000000000000000000, 1.000000000000000000 ) ) ;
#729 = DIRECTION ( 'NONE',  ( 0.000000000000000000, 0.000000000000000000, -1.000000000000000000 ) ) ;
#730 = DIRECTION ( 'NONE',  ( -0.000000000000000000, -1.000000000000000000, -0.000000000000000000 ) ) ;
#731 = CARTESIAN_POINT ( 'NONE',  ( 7.143010269575600368, -13.70175065102395706, 0.6871907070005838225 ) ) ;
#732 = DIRECTION ( 'NONE',  ( 0.000000000000000000, 1.000000000000000000, 0.000000000000000000 ) ) ;
#733 = CARTESIAN_POINT ( 'NONE',  ( 2.121784821875004390, -17.10424616687832966, -6.553150170094818705 ) ) ;
#734 = ADVANCED_FACE ( 'NONE', ( #5775 ), #14125, .F. ) ;
#735 = ORIENTED_EDGE ( 'NONE', *, *, #4911, .T. ) ;
#736 = DIRECTION ( 'NONE',  ( 0.000000000000000000, 0.000000000000000000, -1.000000000000000000 ) ) ;
#737 = CARTESIAN_POINT ( 'NONE',  ( 2.000000000000004441, -20.26142594620695192, -10.69431187202529010 ) ) ;
#738 = ORIENTED_EDGE ( 'NONE', *, *, #3822, .F. ) ;
#739 = ORIENTED_EDGE ( 'NONE', *, *, #2645, .F. ) ;
#740 = CARTESIAN_POINT ( 'NONE',  ( -4.000000000000000888, -21.39983167247694240, -6.280646880243780039 ) ) ;
#741 = FILL_AREA_STYLE_COLOUR ( '', #3929 ) ;
#742 =( NAMED_UNIT ( * ) PLANE_ANGLE_UNIT ( ) SI_UNIT ( $, .RADIAN. ) );
#743 = CARTESIAN_POINT ( 'NONE',  ( 3.673772985318163098, 25.50319992234354416, -2.599342558261029001 ) ) ;
#744 = CARTESIAN_POINT ( 'NONE',  ( -2.211161402132838738, 39.12819992234354771, 2.942372952327218183 ) ) ;
#745 = CARTESIAN_POINT ( 'NONE',  ( 1.593127413382953383, 17.87819992234354416, -2.091722143975172532 ) ) ;
#746 = ORIENTED_EDGE ( 'NONE', *, *, #4495, .T. ) ;
#747 = CARTESIAN_POINT ( 'NONE',  ( 1.444289557195957086, 37.75319992234354771, -4.262301884875733471 ) ) ;
#748 = CARTESIAN_POINT ( 'NONE',  ( -5.279047395330986450E-15, -25.89313373868122881, -4.645111455626608432 ) ) ;
#749 = ORIENTED_EDGE ( 'NONE', *, *, #8614, .F. ) ;
#750 = LINE ( 'NONE', #16234, #7968 ) ;
#751 = CARTESIAN_POINT ( 'NONE',  ( 3.518350579753631191, 34.37180007765648071, 1.080741659609802285 ) ) ;
#752 = DIRECTION ( 'NONE',  ( 0.000000000000000000, -1.000000000000000000, 0.000000000000000000 ) ) ;
#753 = CARTESIAN_POINT ( 'NONE',  ( -2.121784821874996396, -16.77085486324927999, -6.077018044351843784 ) ) ;
#754 = CARTESIAN_POINT ( 'NONE',  ( 2.121784821875004390, -21.23399650860583066, -12.45104488897558248 ) ) ;
#755 = EDGE_CURVE ( 'NONE', #12418, #4334, #3095, .T. ) ;
#756 = CARTESIAN_POINT ( 'NONE',  ( 3.999999999999993339, 7.428752623566170548E-15, -30.00000000000000000 ) ) ;
#757 = EDGE_LOOP ( 'NONE', ( #3139, #14699 ) ) ;
#758 = CARTESIAN_POINT ( 'NONE',  ( -2.978814741686234946, -10.00000000000083844, 22.09987478886784018 ) ) ;
#759 = CARTESIAN_POINT ( 'NONE',  ( 0.3999999999999975797, 0.000000000000000000, 0.000000000000000000 ) ) ;
#760 = FACE_OUTER_BOUND ( 'NONE', #70, .T. ) ;
#761 = CARTESIAN_POINT ( 'NONE',  ( 4.243569643749996345, -28.38075870064580286, -11.97895378909399078 ) ) ;
#762 = ORIENTED_EDGE ( 'NONE', *, *, #13111, .F. ) ;
#763 = CARTESIAN_POINT ( 'NONE',  ( -1.027846397803611866, 25.00319992234354416, -3.346150245485499219 ) ) ;
#764 = DIRECTION ( 'NONE',  ( 1.000000000000000000, 0.000000000000000000, 0.000000000000000000 ) ) ;
#765 = CARTESIAN_POINT ( 'NONE',  ( 4.243569643750003451, -19.64561992126190049, -8.046862975983790633 ) ) ;
#766 = CARTESIAN_POINT ( 'NONE',  ( -2.518350579753628526, 25.62180007765648426, -0.7558219633769075463 ) ) ;
#767 = CARTESIAN_POINT ( 'NONE',  ( 4.499999999999999112, 15.75319992234354416, 0.05647727720528474687 ) ) ;
#768 = CARTESIAN_POINT ( 'NONE',  ( 4.243569643750003451, -23.80763393753414903, -13.99083499735581171 ) ) ;
#769 = CARTESIAN_POINT ( 'NONE',  ( 3.999999999999996447, -27.83000583821450036, -11.43756939096804714 ) ) ;
#770 = CARTESIAN_POINT ( 'NONE',  ( 4.243569643750000786, -21.19011778828857118, -5.981144414553994260 ) ) ;
#771 = CARTESIAN_POINT ( 'NONE',  ( 1.027846397803542144, 16.24680007765647716, -3.346150245485522312 ) ) ;
#772 = CARTESIAN_POINT ( 'NONE',  ( 9.000000000000000000, 34.19999999999999574, -2.500000000000001332 ) ) ;
#773 = CARTESIAN_POINT ( 'NONE',  ( 4.000000000000000888, -26.94918369417327142, -14.20594290873980192 ) ) ;
#774 = FACE_OUTER_BOUND ( 'NONE', #8330, .T. ) ;
#775 = EDGE_LOOP ( 'NONE', ( #10453, #6606, #13929, #968 ) ) ;
#776 = ORIENTED_EDGE ( 'NONE', *, *, #13288, .T. ) ;
#777 = PLANE ( 'NONE',  #10315 ) ;
#778 = EDGE_CURVE ( 'NONE', #16888, #7294, #3002, .T. ) ;
#779 = CARTESIAN_POINT ( 'NONE',  ( 0.000000000000000000, 13.00000000000000178, 6.000000000000000888 ) ) ;
#780 = CARTESIAN_POINT ( 'NONE',  ( 6.428571428571432378, -14.26578344203647752, -2.827263138854379410 ) ) ;
#781 = ORIENTED_EDGE ( 'NONE', *, *, #883, .T. ) ;
#782 = CARTESIAN_POINT ( 'NONE',  ( -2.481649420246391902, 29.62819992234354416, -0.8687765177875723666 ) ) ;
#783 = CARTESIAN_POINT ( 'NONE',  ( -2.121784821874996396, -21.93304279040865623, -13.44938644295279850 ) ) ;
#784 = CARTESIAN_POINT ( 'NONE',  ( -2.864755990943265829, 25.74680007765647716, -2.011557305968488141 ) ) ;
#785 = DIRECTION ( 'NONE',  ( 1.000000000000000000, 0.000000000000000000, -4.336808689942021680E-16 ) ) ;
#786 = EDGE_CURVE ( 'NONE', #17921, #15490, #9461, .T. ) ;
#787 = CARTESIAN_POINT ( 'NONE',  ( 5.562324373799151900, -10.00000000000000000, -9.830817939999416666 ) ) ;
#788 = CARTESIAN_POINT ( 'NONE',  ( -2.121784821874996396, -22.73963465402730577, -14.60131900523419901 ) ) ;
#789 = ADVANCED_FACE ( 'NONE', ( #9941 ), #12905, .F. ) ;
#790 = AXIS2_PLACEMENT_3D ( 'NONE', #12105, #17977, #16580 ) ;
#791 = DIRECTION ( 'NONE',  ( -1.028113302204112171E-14, 0.1129545544106649313, -0.9936001553129349961 ) ) ;
#792 = CARTESIAN_POINT ( 'NONE',  ( -1.071796769724496334, -29.52751773206367147, -10.91439834318392244 ) ) ;
#793 = CYLINDRICAL_SURFACE ( 'NONE', #838, 0.9999999999999991118 ) ;
#794 = AXIS2_PLACEMENT_3D ( 'NONE', #18164, #18343, #14049 ) ;
#795 = CARTESIAN_POINT ( 'NONE',  ( 4.243569643750000786, -23.73894807732350998, -9.621251311363216985 ) ) ;
#796 = ORIENTED_EDGE ( 'NONE', *, *, #7337, .T. ) ;
#797 = DIRECTION ( 'NONE',  ( 0.000000000000000000, 0.000000000000000000, 1.000000000000000000 ) ) ;
#798 = CYLINDRICAL_SURFACE ( 'NONE', #13600, 0.9999999999999991118 ) ;
#799 = CARTESIAN_POINT ( 'NONE',  ( -1.593127413382998459, 28.37180007765648426, -2.091722143975139669 ) ) ;
#800 = ORIENTED_EDGE ( 'NONE', *, *, #7498, .F. ) ;
#801 = CARTESIAN_POINT ( 'NONE',  ( 3.481649420246370141, 26.62180007765648071, -1.193696214020541602 ) ) ;
#802 = EDGE_CURVE ( 'NONE', #17357, #10052, #5688, .T. ) ;
#803 = CARTESIAN_POINT ( 'NONE',  ( -2.000000000000005773, -22.90389237762567021, -2.389191317703265316 ) ) ;
#804 = APPLICATION_PROTOCOL_DEFINITION ( 'draft international standard', 'automotive_design', 1998, #5944 ) ;
#805 = CARTESIAN_POINT ( 'NONE',  ( -3.500000000000000444, 40.00000000000000711, 3.664603343001004987E-14 ) ) ;
#806 = ORIENTED_EDGE ( 'NONE', *, *, #9638, .F. ) ;
#807 = CARTESIAN_POINT ( 'NONE',  ( -4.243569643749998122, -20.10806592306992613, -8.707304311691796528 ) ) ;
#808 = CARTESIAN_POINT ( 'NONE',  ( -3.518350579753630747, 25.62180007765648071, -1.080741659609802729 ) ) ;
#809 = CIRCLE ( 'NONE', #6115, 10.00000000000000000 ) ;
#810 = ORIENTED_EDGE ( 'NONE', *, *, #506, .F. ) ;
#811 = DIRECTION ( 'NONE',  ( -0.000000000000000000, -0.5000000000000002220, -0.8660254037844384856 ) ) ;
#812 = DIRECTION ( 'NONE',  ( -1.000000000000000000, 0.000000000000000000, 4.336808689942021680E-16 ) ) ;
#813 = EDGE_CURVE ( 'NONE', #18256, #8328, #1525, .T. ) ;
#814 = CARTESIAN_POINT ( 'NONE',  ( -2.072127310227394492, -24.23032511484031915, -16.43161913306204980 ) ) ;
#815 = CARTESIAN_POINT ( 'NONE',  ( 7.710291887657668930, -10.24552755907163970, 9.424636009669162817 ) ) ;
#816 = CARTESIAN_POINT ( 'NONE',  ( -2.000000000000005773, -24.51707610556791650, -4.693056443272829448 ) ) ;
#817 = CARTESIAN_POINT ( 'NONE',  ( 2.121784821874994176, -23.21111423883506220, -2.460191299572788814 ) ) ;
#818 = EDGE_CURVE ( 'NONE', #6875, #12310, #1742, .T. ) ;
#819 = ORIENTED_EDGE ( 'NONE', *, *, #9426, .F. ) ;
#820 = LINE ( 'NONE', #12114, #10678 ) ;
#821 = CARTESIAN_POINT ( 'NONE',  ( -4.000000000000004441, -24.36703810445001750, -6.491938924580010983 ) ) ;
#822 = AXIS2_PLACEMENT_3D ( 'NONE', #16795, #15489, #1027 ) ;
#823 = CARTESIAN_POINT ( 'NONE',  ( 3.500000000000000444, 34.24680007765648071, -0.05647727720536935281 ) ) ;
#824 = ORIENTED_EDGE ( 'NONE', *, *, #8075, .T. ) ;
#825 = CIRCLE ( 'NONE', #3186, 2.000000000000001776 ) ;
#826 = ORIENTED_EDGE ( 'NONE', *, *, #2587, .F. ) ;
#827 = CARTESIAN_POINT ( 'NONE',  ( 9.000000000000000000, 18.79999999999999361, -2.500000000000001332 ) ) ;
#828 =( NAMED_UNIT ( * ) PLANE_ANGLE_UNIT ( ) SI_UNIT ( $, .RADIAN. ) );
#829 = CARTESIAN_POINT ( 'NONE',  ( 2.733110507866328920, 33.62819992234354771, 3.862833514489095510 ) ) ;
#830 = CARTESIAN_POINT ( 'NONE',  ( 3.481649420246395010, 35.87819992234354061, 1.193696214020467439 ) ) ;
#831 = CARTESIAN_POINT ( 'NONE',  ( 2.055738996568281518, 25.50319992234354416, -1.423772053676066518 ) ) ;
#832 = EDGE_LOOP ( 'NONE', ( #12160, #80, #2979, #5721 ) ) ;
#833 = CARTESIAN_POINT ( 'NONE',  ( 1.336863392178479160, 21.24680007765647716, -4.297206761780677731 ) ) ;
#834 = CARTESIAN_POINT ( 'NONE',  ( -5.279047395330986450E-15, -24.60258675689138386, -2.802019355976369752 ) ) ;
#835 = ORIENTED_EDGE ( 'NONE', *, *, #17640, .T. ) ;
#836 = TOROIDAL_SURFACE ( 'NONE', #2897, 4.400000000000002132, 0.4000000000000000222 ) ;
#837 = DIRECTION ( 'NONE',  ( -0.000000000000000000, -1.000000000000000000, -0.000000000000000000 ) ) ;
#838 = AXIS2_PLACEMENT_3D ( 'NONE', #6440, #13568, #4956 ) ;
#839 = CARTESIAN_POINT ( 'NONE',  ( 3.500000000000000444, 36.74680007765648071, -0.05647727720536935281 ) ) ;
#840 = ADVANCED_FACE ( 'NONE', ( #315 ), #18327, .F. ) ;
#841 = DIRECTION ( 'NONE',  ( -0.3258630558627232943, 0.000000000000000000, 0.9454169814551713902 ) ) ;
#842 = EDGE_CURVE ( 'NONE', #9790, #6836, #12069, .T. ) ;
#843 = CARTESIAN_POINT ( 'NONE',  ( 4.243569643750003451, -18.61318233583002879, -6.572389296263599689 ) ) ;
#844 = EDGE_CURVE ( 'NONE', #3667, #1028, #3554, .T. ) ;
#845 = CARTESIAN_POINT ( 'NONE',  ( 4.243569643750003451, -22.77519635210228088, -12.51636131763562076 ) ) ;
#846 = CARTESIAN_POINT ( 'NONE',  ( 4.299564228933482956E-15, -23.15635672500629738, -15.76301181529063555 ) ) ;
#847 = ORIENTED_EDGE ( 'NONE', *, *, #6329, .F. ) ;
#848 = CARTESIAN_POINT ( 'NONE',  ( 6.903430137609765538, -10.00000000000000178, 15.77881270003217828 ) ) ;
#849 = SURFACE_SIDE_STYLE ('',( #16621 ) ) ;
#850 = FACE_OUTER_BOUND ( 'NONE', #998, .T. ) ;
#851 = VERTEX_POINT ( 'NONE', #6424 ) ;
#852 = CARTESIAN_POINT ( 'NONE',  ( -2.798362969681409851, 34.75319992234354771, -2.102939460078765421 ) ) ;
#853 = AXIS2_PLACEMENT_3D ( 'NONE', #2448, #17847, #13464 ) ;
#854 = CARTESIAN_POINT ( 'NONE',  ( -4.243569643750000786, -20.51258062284889760, -5.013521062237622949 ) ) ;
#855 = CARTESIAN_POINT ( 'NONE',  ( -2.518350579753628526, 18.12180007765648071, -0.7558219633769075463 ) ) ;
#856 = CARTESIAN_POINT ( 'NONE',  ( -4.481649420246396787, 17.12819992234354416, -1.518615910253363399 ) ) ;
#857 = CARTESIAN_POINT ( 'NONE',  ( 2.000000000000004441, -22.00366437091829397, -13.18248620554634698 ) ) ;
#858 = ORIENTED_EDGE ( 'NONE', *, *, #7727, .T. ) ;
#859 = CARTESIAN_POINT ( 'NONE',  ( -4.243569643749997233, -19.84995652671195998, -8.338685891761748792 ) ) ;
#860 = CARTESIAN_POINT ( 'NONE',  ( 1.444289557196047680, 37.24680007765646650, 4.262301884875704161 ) ) ;
#861 = PRESENTATION_LAYER_ASSIGNMENT (  '', '', ( #563 ) ) ;
#862 = CIRCLE ( 'NONE', #17761, 0.9999999999999991118 ) ;
#863 = DIRECTION ( 'NONE',  ( 0.000000000000000000, 0.000000000000000000, -1.000000000000000000 ) ) ;
#864 = DIRECTION ( 'NONE',  ( 0.000000000000000000, 0.000000000000000000, -1.000000000000000000 ) ) ;
#865 = CARTESIAN_POINT ( 'NONE',  ( 1.071796769724485232, -25.95546013140888064, -5.812971400840699410 ) ) ;
#866 = ORIENTED_EDGE ( 'NONE', *, *, #16394, .T. ) ;
#867 = EDGE_LOOP ( 'NONE', ( #3646, #10246, #14638, #9895 ) ) ;
#868 = CARTESIAN_POINT ( 'NONE',  ( 3.500000000000000444, 19.24680007765648071, -0.05647727720536935281 ) ) ;
#870 = EDGE_CURVE ( 'NONE', #10092, #12622, #898, .T. ) ;
#869 = CARTESIAN_POINT ( 'NONE',  ( 3.579096709490575479E-14, -24.93454924669583406, -4.354959555776423130 ) ) ;
#871 = DIRECTION ( 'NONE',  ( 3.469446951953612217E-16, -0.000000000000000000, 1.000000000000000000 ) ) ;
#872 = ORIENTED_EDGE ( 'NONE', *, *, #16127, .F. ) ;
#873 = CARTESIAN_POINT ( 'NONE',  ( 0.8262555684460829442, 25.25319992234354771, -2.360188852285421302 ) ) ;
#874 = SURFACE_SIDE_STYLE ('',( #12074 ) ) ;
#875 = CARTESIAN_POINT ( 'NONE',  ( -4.243569643749997233, -22.65689621210486138, -12.34741120850101836 ) ) ;
#876 = CARTESIAN_POINT ( 'NONE',  ( 2.211161402132902243, 27.12180007765647360, 2.942372952327172442 ) ) ;
#877 = TOROIDAL_SURFACE ( 'NONE', #14176, 9.000000000000003553, 0.9999999999999991118 ) ;
#878 = DIRECTION ( 'NONE',  ( 0.000000000000000000, 0.000000000000000000, 1.000000000000000000 ) ) ;
#879 = AXIS2_PLACEMENT_3D ( 'NONE', #12311, #1109, #2418 ) ;
#880 = CARTESIAN_POINT ( 'NONE',  ( -1.006530391518317247, -10.00000000000122213, -4.211315095027532429 ) ) ;
#881 = CARTESIAN_POINT ( 'NONE',  ( -4.243569643750000786, -25.70703222455301784, -12.43196676332983408 ) ) ;
#882 = CARTESIAN_POINT ( 'NONE',  ( -9.000000000000003553, 38.59999999999999432, -2.500000000000001776 ) ) ;
#883 = EDGE_CURVE ( 'NONE', #15966, #8825, #1892, .T. ) ;
#884 = CARTESIAN_POINT ( 'NONE',  ( -4.499999999999999112, 22.99680007765647716, 0.05647727720537927543 ) ) ;
#885 = AXIS2_PLACEMENT_3D ( 'NONE', #7012, #8412, #13804 ) ;
#886 = CARTESIAN_POINT ( 'NONE',  ( -4.000000000000000888, -20.17381204048153265, -4.529709386582819519 ) ) ;
#887 = DIRECTION ( 'NONE',  ( -0.000000000000000000, 1.000000000000000000, -0.000000000000000000 ) ) ;
#888 = CARTESIAN_POINT ( 'NONE',  ( -4.243569643749997233, -20.85013043759908413, -9.767082268990684213 ) ) ;
#889 = ORIENTED_EDGE ( 'NONE', *, *, #5357, .T. ) ;
#890 = ADVANCED_FACE ( 'NONE', ( #11889 ), #10502, .F. ) ;
#891 = DIRECTION ( 'NONE',  ( -0.000000000000000000, -1.000000000000000000, -0.000000000000000000 ) ) ;
#892 = FACE_OUTER_BOUND ( 'NONE', #14880, .T. ) ;
#893 = CARTESIAN_POINT ( 'NONE',  ( 2.518350579753628971, 29.37180007765648426, 0.7558219633769073242 ) ) ;
#894 = VERTEX_POINT ( 'NONE', #16173 ) ;
#895 = CARTESIAN_POINT ( 'NONE',  ( 2.115076519116362963, 33.87180007765648071, -3.012182706137107591 ) ) ;
#896 = DIRECTION ( 'NONE',  ( 1.000000000000000000, 0.000000000000000000, -4.336808689942021680E-16 ) ) ;
#897 = ITEM_DEFINED_TRANSFORMATION ( 'NONE', 'NONE', #11598,  #16940 ) ;
#898 = CIRCLE ( 'NONE', #3267, 0.9999999999999991118 ) ;
#899 = DIRECTION ( 'NONE',  ( 0.000000000000000000, 0.8191520442889952403, -0.5735764363510413855 ) ) ;
#900 = ORIENTED_EDGE ( 'NONE', *, *, #12146, .T. ) ;
#901 = CARTESIAN_POINT ( 'NONE',  ( 4.730628863548789710E-15, -19.17657787239343747, -11.64849162045545405 ) ) ;
#902 = CARTESIAN_POINT ( 'NONE',  ( -2.864755990943265829, 25.74680007765647716, -2.011557305968488141 ) ) ;
#903 = COLOUR_RGB ( '',0.8941176470588234615, 0.8941176470588234615, 0.8941176470588234615 ) ;
#904 = VERTEX_POINT ( 'NONE', #11982 ) ;
#905 = DIRECTION ( 'NONE',  ( 1.000000000000000000, 0.000000000000000000, 0.000000000000000000 ) ) ;
#906 = DIRECTION ( 'NONE',  ( 0.000000000000000000, 0.8660254037844380415, -0.5000000000000011102 ) ) ;
#907 = CARTESIAN_POINT ( 'NONE',  ( -9.000000000000001776, 40.79999999999999716, 2.499999999999998224 ) ) ;
#908 = CARTESIAN_POINT ( 'NONE',  ( 9.000000000000005329, 23.19999999999999574, 2.499999999999997335 ) ) ;
#909 = EDGE_CURVE ( 'NONE', #2259, #4661, #14792, .T. ) ;
#910 = DIRECTION ( 'NONE',  ( -0.000000000000000000, -1.000000000000000000, -0.000000000000000000 ) ) ;
#911 = CARTESIAN_POINT ( 'NONE',  ( 4.730628863548789710E-15, -23.01595514321822122, -17.13169061691491279 ) ) ;
#912 = ORIENTED_EDGE ( 'NONE', *, *, #6249, .F. ) ;
#913 = CARTESIAN_POINT ( 'NONE',  ( 2.000000000000004441, -20.51953534256492162, -11.06293029195533784 ) ) ;
#914 = AXIS2_PLACEMENT_3D ( 'NONE', #3726, #9376, #2718 ) ;
#915 = CARTESIAN_POINT ( 'NONE',  ( -1.027846397803541700, 29.99680007765648071, 3.346150245485522312 ) ) ;
#916 = ORIENTED_EDGE ( 'NONE', *, *, #8515, .T. ) ;
#917 = ORIENTED_EDGE ( 'NONE', *, *, #11339, .T. ) ;
#918 = CARTESIAN_POINT ( 'NONE',  ( -5.577813053751546416E-15, -28.80619019206536535, -9.884235854727139170 ) ) ;
#919 = SURFACE_STYLE_USAGE ( .BOTH. , #14844 ) ;
#920 = CARTESIAN_POINT ( 'NONE',  ( 4.518350579753602325, 33.12819992234354771, -1.405661355842793725 ) ) ;
#921 = CARTESIAN_POINT ( 'NONE',  ( -3.500000000000000444, 37.00319992234354061, -0.05647727720529563400 ) ) ;
#922 = CARTESIAN_POINT ( 'NONE',  ( -1.989345975306457071, 29.75319992234354771, -1.515154207786300944 ) ) ;
#923 = EDGE_LOOP ( 'NONE', ( #2456, #2472, #11386, #4432 ) ) ;
#924 = CARTESIAN_POINT ( 'NONE',  ( 4.481649420246366589, 21.62180007765647716, -1.518615910253458212 ) ) ;
#925 = CARTESIAN_POINT ( 'NONE',  ( 4.000000000000003553, -18.58318905575096025, -6.284382248540171467 ) ) ;
#926 = ORIENTED_EDGE ( 'NONE', *, *, #4785, .F. ) ;
#927 = AXIS2_PLACEMENT_3D ( 'NONE', #1459, #7089, #2934 ) ;
#928 = DIRECTION ( 'NONE',  ( -1.000000000000000000, -0.000000000000000000, -0.000000000000000000 ) ) ;
#929 = CARTESIAN_POINT ( 'NONE',  ( -3.518350579753630747, 35.62180007765648782, -1.080741659609802729 ) ) ;
#930 =( BOUNDED_CURVE ( )  B_SPLINE_CURVE ( 2, ( #9246, #10541, #11939, #16216, #3511, #3596, #2401, #14834, #16403 ),
 .UNSPECIFIED., .F., .T. ) 
 B_SPLINE_CURVE_WITH_KNOTS ( ( 3, 2, 2, 2, 3 ),
 ( 0.5086206896551724865, 0.5114942528735632044, 0.5172413793103448620, 0.5229885057471264087, 0.5258620689655172376 ),
 .UNSPECIFIED. ) 
 CURVE ( )  GEOMETRIC_REPRESENTATION_ITEM ( )  RATIONAL_B_SPLINE_CURVE ( ( 0.9330127018922194093, 0.9330127018922206306, 1.000000000000000000, 0.8660254037844387076, 1.000000000000000000, 0.8660254037844387076, 1.000000000000000000, 0.9330127018922194093, 0.9330127018922194093 ) ) 
 REPRESENTATION_ITEM ( '' )  );
#931 = LINE ( 'NONE', #5180, #9055 ) ;
#932 = CARTESIAN_POINT ( 'NONE',  ( 4.243569643750000786, -20.64163532102788778, -5.197830272202643265 ) ) ;
#933 = CARTESIAN_POINT ( 'NONE',  ( 4.243569643749996345, -26.57399292614002562, -9.398624849583658403 ) ) ;
#934 = CARTESIAN_POINT ( 'NONE',  ( 2.659568448039375088, -29.44477373260542663, -12.53330527340647471 ) ) ;
#935 = VERTEX_POINT ( 'NONE', #779 ) ;
#936 = PRODUCT_DEFINITION_CONTEXT ( 'detailed design', #5355, 'design' ) ;
#937 = CARTESIAN_POINT ( 'NONE',  ( -3.772879157352762913, -10.00000000000000178, -12.59063537424807677 ) ) ;
#938 = CARTESIAN_POINT ( 'NONE',  ( -2.000000000000005773, -25.48498634120535655, -6.075375517003743120 ) ) ;
#939 = CARTESIAN_POINT ( 'NONE',  ( -4.000000000000004441, -24.62514750080798720, -6.860557344510057831 ) ) ;
#940 = ORIENTED_EDGE ( 'NONE', *, *, #5873, .T. ) ;
#941 = CARTESIAN_POINT ( 'NONE',  ( 3.481649420246394122, 35.87819992234353350, 1.193696214020467439 ) ) ;
#942 = DIRECTION ( 'NONE',  ( 3.469446951953612217E-16, -0.000000000000000000, 1.000000000000000000 ) ) ;
#943 = CARTESIAN_POINT ( 'NONE',  ( 2.000000000000004441, -24.13306689157648321, -16.22358817097600436 ) ) ;
#944 = CARTESIAN_POINT ( 'NONE',  ( -0.8262555684461330152, 30.99680007765647716, -2.360188852285403982 ) ) ;
#945 = ADVANCED_FACE ( 'NONE', ( #10409 ), #3647, .T. ) ;
#946 = CARTESIAN_POINT ( 'NONE',  ( -1.336863392178569088, 27.50319992234354771, -4.297206761780648421 ) ) ;
#947 = EDGE_CURVE ( 'NONE', #14660, #16355, #5656, .T. ) ;
#948 = CARTESIAN_POINT ( 'NONE',  ( -4.000000000000000888, -24.49714442877256459, -10.70406791940435198 ) ) ;
#949 = ORIENTED_EDGE ( 'NONE', *, *, #17401, .F. ) ;
#950 = EDGE_CURVE ( 'NONE', #1446, #1376, #14215, .T. ) ;
#951 = CARTESIAN_POINT ( 'NONE',  ( 4.243569643749996345, -21.92802379169658877, -2.763493290842798267 ) ) ;
#952 = VECTOR ( 'NONE', #4659, 1000.000000000000000 ) ;
#953 = CIRCLE ( 'NONE', #984, 8.000000000000000000 ) ;
#954 = CARTESIAN_POINT ( 'NONE',  ( 2.733110507866247652, 36.37180007765647360, -3.862833514489153686 ) ) ;
#955 = CARTESIAN_POINT ( 'NONE',  ( 1.533898589781675205E-14, -27.45111586048108521, -7.948989149087622330 ) ) ;
#956 =( GEOMETRIC_REPRESENTATION_CONTEXT ( 3 ) GLOBAL_UNCERTAINTY_ASSIGNED_CONTEXT ( ( #17928 ) ) GLOBAL_UNIT_ASSIGNED_CONTEXT ( ( #7948, #17991, #15201 ) ) REPRESENTATION_CONTEXT ( 'NONE', 'WORKASPACE' ) );
#957 = ADVANCED_FACE ( 'NONE', ( #13377 ), #17676, .T. ) ;
#958 = DIRECTION ( 'NONE',  ( 0.000000000000000000, 0.000000000000000000, 1.000000000000000000 ) ) ;
#959 = CARTESIAN_POINT ( 'NONE',  ( 1.300000000000000044, 1.443375672974065216, 7.222237291452134449E-31 ) ) ;
#960 = DIRECTION ( 'NONE',  ( -1.000000000000000000, 0.000000000000000000, 4.336808689942021680E-16 ) ) ;
#961 = EDGE_LOOP ( 'NONE', ( #16910, #10250, #7255 ) ) ;
#962 = ORIENTED_EDGE ( 'NONE', *, *, #14291, .T. ) ;
#963 = CARTESIAN_POINT ( 'NONE',  ( -1.135272562821090014, 18.49680007765648071, -3.311245368580554072 ) ) ;
#964 = EDGE_CURVE ( 'NONE', #3700, #5980, #16269, .T. ) ;
#965 = AXIS2_PLACEMENT_3D ( 'NONE', #17029, #8642, #1809 ) ;
#966 = LINE ( 'NONE', #2454, #5685 ) ;
#967 = CARTESIAN_POINT ( 'NONE',  ( 7.406012110500714840, -12.49260087798120367, 8.584195667863683710 ) ) ;
#968 = ORIENTED_EDGE ( 'NONE', *, *, #11920, .T. ) ;
#969 = AXIS2_PLACEMENT_3D ( 'NONE', #3169, #14578, #16244 ) ;
#970 = CARTESIAN_POINT ( 'NONE',  ( -1.027846397803611866, 15.00319992234354594, -3.346150245485499219 ) ) ;
#971 = CARTESIAN_POINT ( 'NONE',  ( 4.243569643750003451, -22.74293267755752623, -12.47028401514436169 ) ) ;
#972 = CARTESIAN_POINT ( 'NONE',  ( 2.115076519116362963, 31.37180007765647716, -3.012182706137107147 ) ) ;
#973 = CARTESIAN_POINT ( 'NONE',  ( 3.500000000000000444, 20.75319992234354416, 0.05647727720529520379 ) ) ;
#974 = CARTESIAN_POINT ( 'NONE',  ( 2.798362969681409851, 18.50319992234354771, 2.102939460078764977 ) ) ;
#975 = CYLINDRICAL_SURFACE ( 'NONE', #13734, 4.000000000000000000 ) ;
#976 = FACE_OUTER_BOUND ( 'NONE', #6780, .T. ) ;
#977 = CARTESIAN_POINT ( 'NONE',  ( 4.243569643750000786, -26.09419631908997772, -12.98489439322490213 ) ) ;
#978 = MECHANICAL_DESIGN_GEOMETRIC_PRESENTATION_REPRESENTATION (  '', ( #16081 ), #688 ) ;
#979 = DIRECTION ( 'NONE',  ( -0.000000000000000000, -0.000000000000000000, 1.000000000000000000 ) ) ;
#980 = CARTESIAN_POINT ( 'NONE',  ( -2.829195390882805139, 23.37180007765647716, -3.793023760679206102 ) ) ;
#981 = CARTESIAN_POINT ( 'NONE',  ( -1.734723475976807094E-15, 40.79999999999999716, -2.500000000000000000 ) ) ;
#982 = DIRECTION ( 'NONE',  ( 3.469446951953612217E-16, -0.000000000000000000, 1.000000000000000000 ) ) ;
#983 = CARTESIAN_POINT ( 'NONE',  ( 4.243569643750003451, -19.38751052490393434, -7.678244556053742897 ) ) ;
#984 = AXIS2_PLACEMENT_3D ( 'NONE', #4156, #12407, #11016 ) ;
#985 = VERTEX_POINT ( 'NONE', #501 ) ;
#986 = CARTESIAN_POINT ( 'NONE',  ( -1.071796769724487675, -23.59652146720896582, -16.39163221450554531 ) ) ;
#987 = CARTESIAN_POINT ( 'NONE',  ( -1.989345975306426206, 40.24680007765648071, 1.515154207786343799 ) ) ;
#988 = CARTESIAN_POINT ( 'NONE',  ( 3.064181913176683203, -21.66367673124435100, -2.174801284911689336 ) ) ;
#989 = CARTESIAN_POINT ( 'NONE',  ( -2.798362969681365886, 27.74680007765648071, 2.102939460078824929 ) ) ;
#990 = CYLINDRICAL_SURFACE ( 'NONE', #8370, 0.9999999999999991118 ) ;
#991 = VECTOR ( 'NONE', #7879, 1000.000000000000000 ) ;
#992 =( NAMED_UNIT ( * ) SI_UNIT ( $, .STERADIAN. ) SOLID_ANGLE_UNIT ( ) );
#993 = AXIS2_PLACEMENT_3D ( 'NONE', #11771, #1974, #13258 ) ;
#994 = FACE_OUTER_BOUND ( 'NONE', #4572, .T. ) ;
#995 = ORIENTED_EDGE ( 'NONE', *, *, #17161, .F. ) ;
#996 = CARTESIAN_POINT ( 'NONE',  ( -2.121784821874996396, -18.09366551958387248, -7.966187446493337987 ) ) ;
#997 = CARTESIAN_POINT ( 'NONE',  ( -2.798362969681365886, 27.74680007765648071, 2.102939460078824929 ) ) ;
#998 = EDGE_LOOP ( 'NONE', ( #10590, #3435, #5889, #4242 ) ) ;
#999 = CARTESIAN_POINT ( 'NONE',  ( -15.00000000000000178, 13.00000000000000178, 24.99999999999999645 ) ) ;
#1000 = CARTESIAN_POINT ( 'NONE',  ( 4.243569643750003451, -25.06591724477924288, -15.78784979451479309 ) ) ;
#1001 = CARTESIAN_POINT ( 'NONE',  ( 3.220835151890553583, -25.02781588011482938, -15.95816000315516270 ) ) ;
#1002 = AXIS2_PLACEMENT_3D ( 'NONE', #4784, #16114, #17423 ) ;
#1003 = CARTESIAN_POINT ( 'NONE',  ( 10.00272540370463226, -9.915619283365160186, 6.515181925709914168 ) ) ;
#1004 = CARTESIAN_POINT ( 'NONE',  ( -1.734723475976807094E-15, 27.59999999999999432, -12.50000000000000000 ) ) ;
#1005 = CARTESIAN_POINT ( 'NONE',  ( 2.121784821875004390, -23.78282679764076590, -16.09115178578480254 ) ) ;
#1006 = VERTEX_POINT ( 'NONE', #6050 ) ;
#1007 = DIRECTION ( 'NONE',  ( -0.000000000000000000, -1.000000000000000000, -0.000000000000000000 ) ) ;
#1008 = CARTESIAN_POINT ( 'NONE',  ( -4.000000000000004441, -24.10892870809205135, -6.123320504649964136 ) ) ;
#1009 = CARTESIAN_POINT ( 'NONE',  ( -1.027846397803541700, 34.99680007765648071, 3.346150245485522312 ) ) ;
#1010 = ORIENTED_EDGE ( 'NONE', *, *, #1403, .F. ) ;
#1011 = ORIENTED_EDGE ( 'NONE', *, *, #17505, .F. ) ;
#1012 = CARTESIAN_POINT ( 'NONE',  ( -1.071796769724486786, -17.91811474733365372, -8.282026976044495115 ) ) ;
#1013 = CARTESIAN_POINT ( 'NONE',  ( 2.829195390882724759, 30.37819992234354061, -3.793023760679264278 ) ) ;
#1014 = DIRECTION ( 'NONE',  ( 0.000000000000000000, 0.4999999999999990008, -0.8660254037844391517 ) ) ;
#1015 = CARTESIAN_POINT ( 'NONE',  ( 2.500000000000001332, 25.75319992234354771, 0.05647727720530566764 ) ) ;
#1016 = TOROIDAL_SURFACE ( 'NONE', #15523, 2.200000000000000178, 0.2000000000000000111 ) ;
#1017 = ORIENTED_EDGE ( 'NONE', *, *, #16720, .F. ) ;
#1018 = CARTESIAN_POINT ( 'NONE',  ( -1.444289557196047014, 23.49680007765647716, -4.262301884875704161 ) ) ;
#1019 = EDGE_CURVE ( 'NONE', #5846, #2315, #17393, .T. ) ;
#1020 = CARTESIAN_POINT ( 'NONE',  ( -4.000000000000004441, -22.49574498014980151, -3.819455379080400004 ) ) ;
#1021 = EDGE_LOOP ( 'NONE', ( #11107, #14324, #7812, #9618 ) ) ;
#1022 = DIRECTION ( 'NONE',  ( -0.000000000000000000, 1.000000000000000000, -0.000000000000000000 ) ) ;
#1023 = CARTESIAN_POINT ( 'NONE',  ( 2.864755990943265829, 34.49680007765648071, 2.011557305968487697 ) ) ;
#1024 = DIRECTION ( 'NONE',  ( 0.000000000000000000, 0.000000000000000000, 1.000000000000000000 ) ) ;
#1025 = CARTESIAN_POINT ( 'NONE',  ( 4.730628863548789710E-15, -16.30511083791103744, -7.547611698733672547 ) ) ;
#1026 = CARTESIAN_POINT ( 'NONE',  ( -4.243569643750005227, -24.33704482437095251, -6.203931876856584537 ) ) ;
#1027 = DIRECTION ( 'NONE',  ( 0.000000000000000000, 0.000000000000000000, 1.000000000000000000 ) ) ;
#1028 = VERTEX_POINT ( 'NONE', #11795 ) ;
#1029 = CARTESIAN_POINT ( 'NONE',  ( 4.000000000000000000, -1.759474945355388176, -3.047499999999998099 ) ) ;
#1030 = SURFACE_STYLE_USAGE ( .BOTH. , #14955 ) ;
#1031 =( NAMED_UNIT ( * ) SI_UNIT ( $, .STERADIAN. ) SOLID_ANGLE_UNIT ( ) );
#1032 = ORIENTED_EDGE ( 'NONE', *, *, #12585, .T. ) ;
#1033 = CARTESIAN_POINT ( 'NONE',  ( -0.05938372350920063936, 33.87819992234354771, 3.680117784833935701 ) ) ;
#1034 = CARTESIAN_POINT ( 'NONE',  ( -0.05938372350920064630, 21.37819992234354061, 3.680117784833935701 ) ) ;
#1035 = CARTESIAN_POINT ( 'NONE',  ( -1.999999999999996225, -24.09004865885014723, -16.16215176765433270 ) ) ;
#1036 = CARTESIAN_POINT ( 'NONE',  ( 1.989345975306426206, 31.49680007765648071, -1.515154207786343799 ) ) ;
#1037 = CARTESIAN_POINT ( 'NONE',  ( 4.499999999999999112, 23.25319992234354416, 0.05647727720528474687 ) ) ;
#1038 = UNCERTAINTY_MEASURE_WITH_UNIT (LENGTH_MEASURE( 1.000000000000000082E-05 ), #1383, 'distance_accuracy_value', 'NONE');
#1039 = CARTESIAN_POINT ( 'NONE',  ( 4.000000000000003553, -23.22915819019439709, -12.91951380728103160 ) ) ;
#1040 =( BOUNDED_CURVE ( )  B_SPLINE_CURVE ( 2, ( #17747, #2068, #2251, #9184, #3626, #939, #15037, #13627, #3540 ),
 .UNSPECIFIED., .F., .T. ) 
 B_SPLINE_CURVE_WITH_KNOTS ( ( 3, 2, 2, 2, 3 ),
 ( 0.5603448275862069616, 0.5632183908045976795, 0.5689655172413793371, 0.5747126436781608838, 0.5775862068965517127 ),
 .UNSPECIFIED. ) 
 CURVE ( )  GEOMETRIC_REPRESENTATION_ITEM ( )  RATIONAL_B_SPLINE_CURVE ( ( 0.9330127018922194093, 0.9330127018922206306, 1.000000000000000000, 0.8660254037844387076, 1.000000000000000000, 0.8660254037844387076, 1.000000000000000000, 0.9330127018922194093, 0.9330127018922194093 ) ) 
 REPRESENTATION_ITEM ( '' )  );
#1041 = ORIENTED_EDGE ( 'NONE', *, *, #17682, .F. ) ;
#1042 = CARTESIAN_POINT ( 'NONE',  ( -4.243569643749997233, -18.30130014856414533, -6.126975372181463264 ) ) ;
#1043 = CARTESIAN_POINT ( 'NONE',  ( -4.481649420246366589, 35.37180007765647360, 1.518615910253458878 ) ) ;
#1044 = CARTESIAN_POINT ( 'NONE',  ( 8.500000000000019540, 0.000000000000000000, -20.49999999999998934 ) ) ;
#1045 = CARTESIAN_POINT ( 'NONE',  ( -5.330712181944246111E-15, -28.33358195679832292, -7.640088304762238103 ) ) ;
#1046 = CARTESIAN_POINT ( 'NONE',  ( 1.999999999999994449, -29.05549965749059638, -11.17459699270273354 ) ) ;
#1047 = EDGE_CURVE ( 'NONE', #3748, #10497, #9446, .T. ) ;
#1048 = ADVANCED_FACE ( 'NONE', ( #15059 ), #13745, .F. ) ;
#1049 = CARTESIAN_POINT ( 'NONE',  ( 3.999999999999996447, -23.24856405356550226, -4.894592438216466057 ) ) ;
#1050 = ADVANCED_FACE ( 'NONE', ( #6785 ), #12440, .T. ) ;
#1051 = CARTESIAN_POINT ( 'NONE',  ( 0.000000000000000000, 5.977523610840987267, 32.81826849749789687 ) ) ;
#1052 = VERTEX_POINT ( 'NONE', #12255 ) ;
#1053 = ORIENTED_EDGE ( 'NONE', *, *, #3090, .F. ) ;
#1054 = DIRECTION ( 'NONE',  ( -0.000000000000000000, 1.000000000000000000, -0.000000000000000000 ) ) ;
#1055 = CARTESIAN_POINT ( 'NONE',  ( -1.734723475976807094E-15, 40.79999999999999716, -11.50000000000000178 ) ) ;
#1056 = CARTESIAN_POINT ( 'NONE',  ( 0.000000000000000000, 33.00000000000000000, -4.000000000000000888 ) ) ;
#1057 = CARTESIAN_POINT ( 'NONE',  ( 3.999999999999996447, -26.02324006370871956, -8.857240451457712993 ) ) ;
#1058 = VERTEX_POINT ( 'NONE', #8272 ) ;
#1059 = CARTESIAN_POINT ( 'NONE',  ( 1.593127413382953383, 32.87819992234354771, -2.091722143975172532 ) ) ;
#1060 = CARTESIAN_POINT ( 'NONE',  ( 2.121784821875004390, -21.45984223041904926, -12.77358600641437469 ) ) ;
#1061 = CARTESIAN_POINT ( 'NONE',  ( -2.798362969681365886, 32.74680007765648071, 2.102939460078824929 ) ) ;
#1062 = CARTESIAN_POINT ( 'NONE',  ( -3.518350579753605434, 24.37819992234353705, 1.080741659609877781 ) ) ;
#1063 = DIRECTION ( 'NONE',  ( 0.000000000000000000, -1.000000000000000000, 0.000000000000000000 ) ) ;
#1064 = DIRECTION ( 'NONE',  ( -0.000000000000000000, -0.5735764363510414965, -0.8191520442889950182 ) ) ;
#1065 = VECTOR ( 'NONE', #8366, 1000.000000000000000 ) ;
#1066 = CARTESIAN_POINT ( 'NONE',  ( -2.121784821875005722, -27.38388281328888141, -8.419522421775232246 ) ) ;
#1067 = CARTESIAN_POINT ( 'NONE',  ( -3.500000000000000444, 15.00000000000001243, 3.664603343001004987E-14 ) ) ;
#1068 = CARTESIAN_POINT ( 'NONE',  ( -4.481649420246366589, 22.87180007765647360, 1.518615910253458878 ) ) ;
#1069 = CARTESIAN_POINT ( 'NONE',  ( -1.071796769724505882, -17.46642330441216018, -7.636944742173667144 ) ) ;
#1070 = EDGE_CURVE ( 'NONE', #12491, #16354, #8084, .T. ) ;
#1071 = DIRECTION ( 'NONE',  ( -0.000000000000000000, 1.000000000000000000, -0.000000000000000000 ) ) ;
#1072 = CARTESIAN_POINT ( 'NONE',  ( 2.121784821875004390, -19.39496705955529876, -9.824638646973991030 ) ) ;
#1073 = AXIS2_PLACEMENT_3D ( 'NONE', #1154, #15068, #6797 ) ;
#1074 = CARTESIAN_POINT ( 'NONE',  ( 8.499999999999994671, 13.00000000000000178, 18.35000000000000142 ) ) ;
#1075 = CYLINDRICAL_SURFACE ( 'NONE', #5257, 6.000000000000000888 ) ;
#1076 = CARTESIAN_POINT ( 'NONE',  ( -2.481649420246391902, 14.62819992234354594, -0.8687765177875723666 ) ) ;
#1077 = VECTOR ( 'NONE', #14132, 1000.000000000000000 ) ;
#1078 = CARTESIAN_POINT ( 'NONE',  ( 13.00000000000000178, 15.00000000000000178, -25.00000000000000355 ) ) ;
#1079 = FACE_OUTER_BOUND ( 'NONE', #12862, .T. ) ;
#1080 = FACE_OUTER_BOUND ( 'NONE', #10617, .T. ) ;
#1081 = CONTEXT_DEPENDENT_SHAPE_REPRESENTATION ( #1227, #13259 ) ;
#1082 = LINE ( 'NONE', #2294, #16709 ) ;
#1083 = VERTEX_POINT ( 'NONE', #5400 ) ;
#1084 = CARTESIAN_POINT ( 'NONE',  ( -5.330712181944246111E-15, -25.52664227140541087, -3.631362988022969862 ) ) ;
#1085 = CARTESIAN_POINT ( 'NONE',  ( -3.481649420246369697, 27.87180007765647360, 1.193696214020542490 ) ) ;
#1086 = EDGE_LOOP ( 'NONE', ( #5094, #15217, #16916, #17972 ) ) ;
#1087 = DIRECTION ( 'NONE',  ( -0.000000000000000000, -0.5735764363510414965, -0.8191520442889950182 ) ) ;
#1088 = AXIS2_PLACEMENT_3D ( 'NONE', #8564, #7176, #1540 ) ;
#1089 = CARTESIAN_POINT ( 'NONE',  ( 4.243569643749997233, -28.60660442245902502, -12.30149490653278121 ) ) ;
#1090 = FACE_OUTER_BOUND ( 'NONE', #15810, .T. ) ;
#1091 = CARTESIAN_POINT ( 'NONE',  ( 1.300000000000000044, -0.7216878364870317197, -1.250000000000000000 ) ) ;
#1092 = CARTESIAN_POINT ( 'NONE',  ( -4.243569643750005227, -28.43453149155370241, -12.05574929324608924 ) ) ;
#1093 = ORIENTED_EDGE ( 'NONE', *, *, #9929, .T. ) ;
#1094 = FACE_OUTER_BOUND ( 'NONE', #5867, .T. ) ;
#1095 = CARTESIAN_POINT ( 'NONE',  ( 1.999999999999994449, -25.24838606191550028, -5.737475299741293888 ) ) ;
#1096 = CARTESIAN_POINT ( 'NONE',  ( 2.518350579753628971, 16.87180007765648071, 0.7558219633769073242 ) ) ;
#1097 = ORIENTED_EDGE ( 'NONE', *, *, #8515, .F. ) ;
#1098 = CARTESIAN_POINT ( 'NONE',  ( 1.071796769724495224, -22.90977402936716345, -15.41085523001650515 ) ) ;
#1099 = FILL_AREA_STYLE ('',( #8400 ) ) ;
#1100 = CARTESIAN_POINT ( 'NONE',  ( -2.829195390882724315, 36.62819992234354771, 3.793023760679264722 ) ) ;
#1101 = CARTESIAN_POINT ( 'NONE',  ( -2.000000000000005773, -23.16200177398363991, -2.757809737633313940 ) ) ;
#1102 = AXIS2_PLACEMENT_3D ( 'NONE', #5132, #6527, #3742 ) ;
#1103 = CARTESIAN_POINT ( 'NONE',  ( 0.05938372350921204690, 27.62819992234354416, -2.628655560595669183 ) ) ;
#1104 = EDGE_LOOP ( 'NONE', ( #16203, #4829, #9327, #10957 ) ) ;
#1105 = CARTESIAN_POINT ( 'NONE',  ( 4.243569643749997233, -27.34832111521393117, -10.50448010937379983 ) ) ;
#1106 = CARTESIAN_POINT ( 'NONE',  ( 4.499999999999999112, 24.24680007765647716, -0.05647727720537982360 ) ) ;
#1107 = CARTESIAN_POINT ( 'NONE',  ( 4.000000000000000888, -21.27077697429796288, -6.096337670278750842 ) ) ;
#1108 = VERTEX_POINT ( 'NONE', #15332 ) ;
#1109 = DIRECTION ( 'NONE',  ( 1.000000000000000000, 0.000000000000000000, 0.000000000000000000 ) ) ;
#1110 = EDGE_CURVE ( 'NONE', #3352, #16039, #15735, .T. ) ;
#1111 = FILL_AREA_STYLE ('',( #9079 ) ) ;
#1112 = DIRECTION ( 'NONE',  ( -0.000000000000000000, -1.000000000000000000, -0.000000000000000000 ) ) ;
#1113 = ADVANCED_FACE ( 'NONE', ( #1240 ), #4479, .T. ) ;
#1114 = DIRECTION ( 'NONE',  ( 0.000000000000000000, -0.000000000000000000, 1.000000000000000000 ) ) ;
#1115 = AXIS2_PLACEMENT_3D ( 'NONE', #2304, #910, #3862 ) ;
#1116 = CARTESIAN_POINT ( 'NONE',  ( -2.121784821875005722, -26.09333583149904001, -6.576430322124992678 ) ) ;
#1117 = EDGE_CURVE ( 'NONE', #15867, #2086, #9221, .T. ) ;
#1118 = DIRECTION ( 'NONE',  ( -0.000000000000000000, 1.000000000000000000, -0.000000000000000000 ) ) ;
#1119 = EDGE_CURVE ( 'NONE', #2412, #4161, #3603, .T. ) ;
#1120 = ORIENTED_EDGE ( 'NONE', *, *, #4909, .T. ) ;
#1121 = CARTESIAN_POINT ( 'NONE',  ( 4.000000000000000888, -24.17450768403005767, -10.24329489549855410 ) ) ;
#1122 = DIRECTION ( 'NONE',  ( -1.000000000000000000, -0.000000000000000000, 8.673617379884034239E-17 ) ) ;
#1123 = CARTESIAN_POINT ( 'NONE',  ( -2.115076519116362519, 17.62180007765647716, 3.012182706137108035 ) ) ;
#1124 = ADVANCED_FACE ( 'NONE', ( #3731 ), #12345, .F. ) ;
#1125 = ORIENTED_EDGE ( 'NONE', *, *, #2773, .F. ) ;
#1126 = CARTESIAN_POINT ( 'NONE',  ( -3.518350579753605434, 34.37819992234354771, 1.080741659609877781 ) ) ;
#1127 = CARTESIAN_POINT ( 'NONE',  ( -1.135272562821019626, 24.00319992234354416, 3.311245368580577164 ) ) ;
#1128 = CARTESIAN_POINT ( 'NONE',  ( 4.243569643750000786, -20.12541652831194838, -4.460593432342547793 ) ) ;
#1129 = CARTESIAN_POINT ( 'NONE',  ( -0.7188294034286043521, 32.49680007765648782, 2.395093729190366005 ) ) ;
#1130 = CARTESIAN_POINT ( 'NONE',  ( 4.481649420246397675, 28.37819992234355126, 1.518615910253363177 ) ) ;
#1131 = VECTOR ( 'NONE', #12180, 1000.000000000000000 ) ;
#1132 = CARTESIAN_POINT ( 'NONE',  ( 4.000000000000000888, -24.36808973059358863, -10.51975870943932456 ) ) ;
#1133 = ORIENTED_EDGE ( 'NONE', *, *, #8853, .T. ) ;
#1134 = CARTESIAN_POINT ( 'NONE',  ( 4.243569643749996345, -22.44424258441252817, -3.500730130702893739 ) ) ;
#1135 = CARTESIAN_POINT ( 'NONE',  ( -2.211161402132902243, 25.87180007765647360, -2.942372952327172886 ) ) ;
#1136 = CYLINDRICAL_SURFACE ( 'NONE', #6580, 0.9999999999999991118 ) ;
#1137 = CARTESIAN_POINT ( 'NONE',  ( 4.243569643749997233, -26.02551045887933867, -8.615310707232305631 ) ) ;
#1138 = DIRECTION ( 'NONE',  ( 0.000000000000000000, 0.000000000000000000, -1.000000000000000000 ) ) ;
#1139 = CARTESIAN_POINT ( 'NONE',  ( 1.999999999999994449, -24.21594847648362858, -4.263001620021102944 ) ) ;
#1140 = AXIS2_PLACEMENT_3D ( 'NONE', #6146, #11796, #10410 ) ;
#1141 = DIRECTION ( 'NONE',  ( -0.000000000000000000, -1.000000000000000000, -0.000000000000000000 ) ) ;
#1142 = EDGE_LOOP ( 'NONE', ( #18109, #926 ) ) ;
#1143 = VERTEX_POINT ( 'NONE', #9381 ) ;
#1144 = CARTESIAN_POINT ( 'NONE',  ( 2.798362969681366330, 16.49680007765647716, -2.102939460078824929 ) ) ;
#1145 = CARTESIAN_POINT ( 'NONE',  ( -5.000000000000001776, 0.000000000000000000, -4.999999999999999112 ) ) ;
#1146 = CARTESIAN_POINT ( 'NONE',  ( 1.743066579297358403E-15, -23.41446612136426708, -16.13163023522068684 ) ) ;
#1147 = EDGE_LOOP ( 'NONE', ( #4251, #12196, #15311, #16287 ) ) ;
#1148 = CARTESIAN_POINT ( 'NONE',  ( 1.593127413382953383, 37.87819992234354771, -2.091722143975172532 ) ) ;
#1149 = CARTESIAN_POINT ( 'NONE',  ( 4.243569643749996345, -26.02551045887933867, -8.615310707232305631 ) ) ;
#1150 = CARTESIAN_POINT ( 'NONE',  ( 2.798362969681366330, 28.99680007765647716, -2.102939460078824929 ) ) ;
#1151 =( BOUNDED_CURVE ( )  B_SPLINE_CURVE ( 2, ( #12526, #8775, #13048, #4610, #15508, #1758, #16816, #5484, #4088 ),
 .UNSPECIFIED., .F., .F. ) 
 B_SPLINE_CURVE_WITH_KNOTS ( ( 3, 2, 2, 2, 3 ),
 ( 0.8189655172413793371, 0.8218390804597701660, 0.8275862068965517127, 0.8333333333333333703, 0.8362068965517241992 ),
 .UNSPECIFIED. ) 
 CURVE ( )  GEOMETRIC_REPRESENTATION_ITEM ( )  RATIONAL_B_SPLINE_CURVE ( ( 0.9330127018922194093, 0.9330127018922194093, 1.000000000000000000, 0.8660254037844387076, 1.000000000000000000, 0.8660254037844387076, 1.000000000000000000, 0.9330127018922180770, 0.9330127018922194093 ) ) 
 REPRESENTATION_ITEM ( '' )  );
#1152 = CARTESIAN_POINT ( 'NONE',  ( 1.027846397803612311, 28.75319992234354416, 3.346150245485499219 ) ) ;
#1153 = DIRECTION ( 'NONE',  ( 0.000000000000000000, 1.000000000000000000, 0.000000000000000000 ) ) ;
#1154 = CARTESIAN_POINT ( 'NONE',  ( -11.99999999999999822, 48.00000000000000000, -15.00000000000000000 ) ) ;
#1155 = CARTESIAN_POINT ( 'NONE',  ( 4.243569643749996345, -26.31588352978205592, -9.030006429653610667 ) ) ;
#1156 = AXIS2_PLACEMENT_3D ( 'NONE', #15509, #1141, #12527 ) ;
#1157 = ADVANCED_FACE ( 'NONE', ( #13647 ), #7441, .T. ) ;
#1158 = CARTESIAN_POINT ( 'NONE',  ( -0.6435590302262776952, -15.45066141473203203, -10.82404826198590797 ) ) ;
#1159 = CARTESIAN_POINT ( 'NONE',  ( -6.158835246850665095E-15, -22.31750118613795664, -14.56500194951122218 ) ) ;
#1160 = AXIS2_PLACEMENT_3D ( 'NONE', #10521, #10428, #524 ) ;
#1161 = DIRECTION ( 'NONE',  ( 0.000000000000000000, 0.9936001553129348851, 0.1129545544106647231 ) ) ;
#1162 = CIRCLE ( 'NONE', #7024, 0.9999999999999991118 ) ;
#1163 = CARTESIAN_POINT ( 'NONE',  ( 4.730628863548789710E-15, -17.59565781970087883, -9.390703798383910339 ) ) ;
#1164 = CARTESIAN_POINT ( 'NONE',  ( -4.000000000000000888, -26.82012899599428124, -14.02163369877478161 ) ) ;
#1165 = CARTESIAN_POINT ( 'NONE',  ( -9.000000000000001776, 25.39999999999999503, 2.499999999999995559 ) ) ;
#1166 = AXIS2_PLACEMENT_3D ( 'NONE', #8962, #12855, #8673 ) ;
#1167 = CARTESIAN_POINT ( 'NONE',  ( -0.7188294034286043521, 39.99680007765647360, 2.395093729190366005 ) ) ;
#1168 = CIRCLE ( 'NONE', #3535, 8.000000000000001776 ) ;
#1169 = CARTESIAN_POINT ( 'NONE',  ( 2.115076519116362963, 36.37180007765648071, -3.012182706137107591 ) ) ;
#1170 = CARTESIAN_POINT ( 'NONE',  ( -1.071796769724505882, -16.88567716190178913, -6.807553296324296177 ) ) ;
#1171 = CARTESIAN_POINT ( 'NONE',  ( -1.244399073187948845, 15.00000000000001243, -3.410710356087081063 ) ) ;
#1172 = EDGE_CURVE ( 'NONE', #1302, #13373, #966, .T. ) ;
#1173 = EDGE_LOOP ( 'NONE', ( #8409, #3595, #9292, #14919 ) ) ;
#1174 = CARTESIAN_POINT ( 'NONE',  ( -4.243569643750000786, -20.80295369375161130, -5.428216784658927985 ) ) ;
#1175 = CARTESIAN_POINT ( 'NONE',  ( 2.864755990943265829, 24.49680007765647716, 2.011557305968487697 ) ) ;
#1176 = EDGE_CURVE ( 'NONE', #10810, #317, #16342, .T. ) ;
#1177 = PRODUCT_DEFINITION_SHAPE ( 'NONE', 'NONE',  #18374 ) ;
#1178 = EDGE_CURVE ( 'NONE', #11085, #1278, #1255, .T. ) ;
#1179 = VECTOR ( 'NONE', #2036, 1000.000000000000000 ) ;
#1180 = CARTESIAN_POINT ( 'NONE',  ( 9.184850993605147944E-16, -10.54254386713301628, 22.30101802474215589 ) ) ;
#1181 = AXIS2_PLACEMENT_3D ( 'NONE', #3701, #16508, #18001 ) ;
#1182 = CARTESIAN_POINT ( 'NONE',  ( 8.500000000000001776, 10.00000000000000000, -20.49999999999999645 ) ) ;
#1183 = DIRECTION ( 'NONE',  ( 0.000000000000000000, 0.000000000000000000, 1.000000000000000000 ) ) ;
#1184 = EDGE_CURVE ( 'NONE', #13534, #6366, #11299, .T. ) ;
#1185 = CARTESIAN_POINT ( 'NONE',  ( 4.000000000000003553, -24.51970517198423849, -14.76260590693127028 ) ) ;
#1186 = CYLINDRICAL_SURFACE ( 'NONE', #15336, 4.000000000000001776 ) ;
#1187 = CARTESIAN_POINT ( 'NONE',  ( 4.243569643750000786, -26.06193264454523018, -12.93881709073364661 ) ) ;
#1188 = ORIENTED_EDGE ( 'NONE', *, *, #10509, .T. ) ;
#1189 = CYLINDRICAL_SURFACE ( 'NONE', #927, 2.149999999999995470 ) ;
#1190 = CARTESIAN_POINT ( 'NONE',  ( -1.999999999999996225, -18.92786073169077454, -8.789783369053376205 ) ) ;
#1191 = CARTESIAN_POINT ( 'NONE',  ( 1.027846397803542144, 38.74680007765647360, -3.346150245485522312 ) ) ;
#1192 = ORIENTED_EDGE ( 'NONE', *, *, #5126, .F. ) ;
#1193 = DIRECTION ( 'NONE',  ( -0.000000000000000000, -0.000000000000000000, -1.000000000000000000 ) ) ;
#1194 = SURFACE_STYLE_FILL_AREA ( #1099 ) ;
#1195 = CIRCLE ( 'NONE', #14837, 6.500000000000000000 ) ;
#1196 = CARTESIAN_POINT ( 'NONE',  ( -2.733110507866328476, 32.37819992234353350, -3.862833514489096398 ) ) ;
#1197 = DIRECTION ( 'NONE',  ( -3.469446951953612217E-16, 0.000000000000000000, -1.000000000000000000 ) ) ;
#1198 = AXIS2_PLACEMENT_3D ( 'NONE', #6842, #12492, #1297 ) ;
#1199 = CARTESIAN_POINT ( 'NONE',  ( -2.518350579753611207, 31.87819992234354416, 0.7558219633769609480 ) ) ;
#1200 = VERTEX_POINT ( 'NONE', #14383 ) ;
#1201 = CARTESIAN_POINT ( 'NONE',  ( -2.121784821875005722, -28.67442979507872636, -10.26261452142547093 ) ) ;
#1202 = CARTESIAN_POINT ( 'NONE',  ( -4.499999999999999112, 27.99680007765647716, 0.05647727720537927543 ) ) ;
#1203 = CARTESIAN_POINT ( 'NONE',  ( -1.999999999999996225, -17.31467700374852470, -6.485918243483816958 ) ) ;
#1204 = VERTEX_POINT ( 'NONE', #11399 ) ;
#1205 = DIRECTION ( 'NONE',  ( -1.000000000000000000, -0.000000000000000000, -0.000000000000000000 ) ) ;
#1206 = CARTESIAN_POINT ( 'NONE',  ( 9.184850993605147944E-16, -8.516114662390016576, 25.19505885429991565 ) ) ;
#1207 = FACE_OUTER_BOUND ( 'NONE', #13649, .T. ) ;
#1208 = AXIS2_PLACEMENT_3D ( 'NONE', #15326, #2625, #8266 ) ;
#1209 = DIRECTION ( 'NONE',  ( 0.000000000000000000, 0.000000000000000000, 1.000000000000000000 ) ) ;
#1210 = CARTESIAN_POINT ( 'NONE',  ( -4.243569643750000786, -22.60971946825739209, -8.008545724169261248 ) ) ;
#1211 = ORIENTED_EDGE ( 'NONE', *, *, #1576, .T. ) ;
#1212 = CARTESIAN_POINT ( 'NONE',  ( 8.500000000000001776, 13.00000000000000000, -22.64999999999999503 ) ) ;
#1213 = ORIENTED_EDGE ( 'NONE', *, *, #4950, .F. ) ;
#1214 = CARTESIAN_POINT ( 'NONE',  ( 4.713407268011036227E-15, -20.32647910872069730, -12.80037636994084416 ) ) ;
#1215 = CARTESIAN_POINT ( 'NONE',  ( 2.399999999999999911, 2.449293598294706414E-16, -2.000000000000000000 ) ) ;
#1216 = FACE_OUTER_BOUND ( 'NONE', #16174, .T. ) ;
#1217 = ORIENTED_EDGE ( 'NONE', *, *, #2834, .F. ) ;
#1218 = CARTESIAN_POINT ( 'NONE',  ( 3.518350579753605434, 38.12819992234354061, -1.080741659609877114 ) ) ;
#1219 = CARTESIAN_POINT ( 'NONE',  ( 2.798362969681409851, 21.00319992234354416, 2.102939460078764977 ) ) ;
#1220 = CARTESIAN_POINT ( 'NONE',  ( 2.121784821874994176, -22.92074116793234140, -2.045495577151484223 ) ) ;
#1221 = CARTESIAN_POINT ( 'NONE',  ( 1.989345975306426206, 33.99680007765647360, -1.515154207786343799 ) ) ;
#1222 = CIRCLE ( 'NONE', #15714, 0.9999999999999991118 ) ;
#1223 = CARTESIAN_POINT ( 'NONE',  ( 0.05938372350919016857, 27.62819992234354416, -4.731580009072201776 ) ) ;
#1224 = UNCERTAINTY_MEASURE_WITH_UNIT (LENGTH_MEASURE( 1.000000000000000082E-05 ), #9211, 'distance_accuracy_value', 'NONE');
#1225 = CARTESIAN_POINT ( 'NONE',  ( -3.999999999999997335, -23.40123112109970194, -13.16525942056773246 ) ) ;
#1226 = ORIENTED_EDGE ( 'NONE', *, *, #6652, .T. ) ;
#1227 =( REPRESENTATION_RELATIONSHIP ('NONE','NONE', #15868, #10770 ) REPRESENTATION_RELATIONSHIP_WITH_TRANSFORMATION ( #9774 )SHAPE_REPRESENTATION_RELATIONSHIP( ) );
#1228 = CARTESIAN_POINT ( 'NONE',  ( -4.000000000000000888, -25.59410936399887504, -12.27069620511382197 ) ) ;
#1229 = CARTESIAN_POINT ( 'NONE',  ( 3.481649420246369697, 21.62180007765647360, -1.193696214020541824 ) ) ;
#1230 = EDGE_CURVE ( 'NONE', #4433, #14538, #8709, .T. ) ;
#1231 = CARTESIAN_POINT ( 'NONE',  ( -1.071796769724496334, -21.07995485342371822, -12.79760262119433634 ) ) ;
#1232 = CARTESIAN_POINT ( 'NONE',  ( -4.243569643750000786, -22.31934639735467840, -7.593850001747957990 ) ) ;
#1233 = VECTOR ( 'NONE', #10797, 1000.000000000000000 ) ;
#1234 = DIRECTION ( 'NONE',  ( 0.000000000000000000, 0.000000000000000000, -1.000000000000000000 ) ) ;
#1235 = FACE_OUTER_BOUND ( 'NONE', #14347, .T. ) ;
#1236 = ORIENTED_EDGE ( 'NONE', *, *, #16460, .F. ) ;
#1237 = ORIENTED_EDGE ( 'NONE', *, *, #11288, .F. ) ;
#1238 = CARTESIAN_POINT ( 'NONE',  ( 2.211161402132902243, 17.12180007765648071, 2.942372952327172442 ) ) ;
#1239 = CYLINDRICAL_SURFACE ( 'NONE', #8162, 0.9999999999999991118 ) ;
#1240 = FACE_OUTER_BOUND ( 'NONE', #5632, .T. ) ;
#1241 = CARTESIAN_POINT ( 'NONE',  ( 5.810221930991194676E-16, -23.67257551772224033, -16.50024865515073458 ) ) ;
#1242 = ORIENTED_EDGE ( 'NONE', *, *, #9556, .F. ) ;
#1243 = CARTESIAN_POINT ( 'NONE',  ( -0.8262555684460826111, 36.50319992234354061, 2.360188852285421302 ) ) ;
#1244 = CARTESIAN_POINT ( 'NONE',  ( -4.243569643750005227, -26.62776571704792161, -9.475420353735755086 ) ) ;
#1245 = CARTESIAN_POINT ( 'NONE',  ( -3.481649420246369697, 30.37180007765647005, 1.193696214020542490 ) ) ;
#1246 = CARTESIAN_POINT ( 'NONE',  ( -3.481649420246394122, 24.62819992234354061, -1.193696214020467883 ) ) ;
#1247 = AXIS2_PLACEMENT_3D ( 'NONE', #6874, #3823, #12532 ) ;
#1248 = CARTESIAN_POINT ( 'NONE',  ( -9.000000000000001776, 16.59999999999999787, 2.499999999999998224 ) ) ;
#1249 = LINE ( 'NONE', #12540, #15570 ) ;
#1250 =( GEOMETRIC_REPRESENTATION_CONTEXT ( 3 ) GLOBAL_UNCERTAINTY_ASSIGNED_CONTEXT ( ( #6593 ) ) GLOBAL_UNIT_ASSIGNED_CONTEXT ( ( #16139, #459, #11752 ) ) REPRESENTATION_CONTEXT ( 'NONE', 'WORKASPACE' ) );
#1251 = CARTESIAN_POINT ( 'NONE',  ( 4.243569643750003451, -22.00086816302836823, -11.41050605784547578 ) ) ;
#1252 = ADVANCED_FACE ( 'NONE', ( #11227 ), #9922, .F. ) ;
#1253 = CARTESIAN_POINT ( 'NONE',  ( 0.2621597573826395799, -10.00000000000313527, -3.075850967169316164 ) ) ;
#1254 = DIRECTION ( 'NONE',  ( 1.000000000000000000, 0.000000000000000000, 0.000000000000000000 ) ) ;
#1255 = CIRCLE ( 'NONE', #17252, 10.00000000000000000 ) ;
#1256 = DIRECTION ( 'NONE',  ( -0.000000000000000000, -1.000000000000000000, -0.000000000000000000 ) ) ;
#1257 =( BOUNDED_CURVE ( )  B_SPLINE_CURVE ( 2, ( #7907, #5128, #10784, #13475, #10511, #6434, #13296, #13562, #10602 ),
 .UNSPECIFIED., .F., .T. ) 
 B_SPLINE_CURVE_WITH_KNOTS ( ( 3, 2, 2, 2, 3 ),
 ( 0.4224137931034482873, 0.4252873563218390607, 0.4310344827586206629, 0.4367816091954023205, 0.4396551724137931494 ),
 .UNSPECIFIED. ) 
 CURVE ( )  GEOMETRIC_REPRESENTATION_ITEM ( )  RATIONAL_B_SPLINE_CURVE ( ( 0.9330127018922194093, 0.9330127018922200755, 1.000000000000000000, 0.8660254037844387076, 1.000000000000000000, 0.8660254037844387076, 1.000000000000000000, 0.9330127018922187432, 0.9330127018922194093 ) ) 
 REPRESENTATION_ITEM ( '' )  );
#1258 = CARTESIAN_POINT ( 'NONE',  ( 2.121784821874994176, -25.24372573515406515, -5.363061356521914291 ) ) ;
#1259 = CARTESIAN_POINT ( 'NONE',  ( -2.000000000000005773, -24.77518550192588620, -5.061674863202877184 ) ) ;
#1260 = COLOUR_RGB ( '',1.000000000000000000, 0.9490196078431372140, 0.9098039215686274384 ) ;
#1261 = CARTESIAN_POINT ( 'NONE',  ( 2.055738996568281518, 15.50319992234354949, -1.423772053676066518 ) ) ;
#1262 = CARTESIAN_POINT ( 'NONE',  ( 2.000000000000004441, -17.61580463283282683, -6.915973066735536356 ) ) ;
#1263 = CARTESIAN_POINT ( 'NONE',  ( -1.027846397803541700, 39.99680007765648071, 3.346150245485522312 ) ) ;
#1264 = CARTESIAN_POINT ( 'NONE',  ( -12.99999999999999822, 48.00000000000000000, -16.00000000000000000 ) ) ;
#1265 = CARTESIAN_POINT ( 'NONE',  ( -1.089585269739795192, 15.00000000000000533, -3.377979775708401355 ) ) ;
#1266 = ORIENTED_EDGE ( 'NONE', *, *, #2716, .F. ) ;
#1267 = AXIS2_PLACEMENT_3D ( 'NONE', #4412, #17046, #60 ) ;
#1268 = CARTESIAN_POINT ( 'NONE',  ( -4.243569643749998122, -19.07562833763805443, -7.232830631971606472 ) ) ;
#1269 = CARTESIAN_POINT ( 'NONE',  ( -3.481649420246369697, 35.37180007765648071, 1.193696214020542490 ) ) ;
#1270 = VECTOR ( 'NONE', #10266, 1000.000000000000000 ) ;
#1271 = CARTESIAN_POINT ( 'NONE',  ( 8.500000000000001776, 14.99364916731036956, -20.49999999999999645 ) ) ;
#1272 = CARTESIAN_POINT ( 'NONE',  ( -4.243569643750000786, -26.96531553179811169, -14.22898156048881724 ) ) ;
#1273 = DIRECTION ( 'NONE',  ( -0.000000000000000000, 1.000000000000000000, -0.000000000000000000 ) ) ;
#1274 = DIRECTION ( 'NONE',  ( 1.000000000000000000, 0.000000000000000000, 0.000000000000000000 ) ) ;
#1275 = DIRECTION ( 'NONE',  ( -0.000000000000000000, 1.000000000000000000, -0.000000000000000000 ) ) ;
#1276 = CARTESIAN_POINT ( 'NONE',  ( 2.121784821875004390, -22.49227981585092095, -14.24805968613456564 ) ) ;
#1277 = EDGE_CURVE ( 'NONE', #11364, #9512, #18161, .T. ) ;
#1278 = VERTEX_POINT ( 'NONE', #1504 ) ;
#1279 = CARTESIAN_POINT ( 'NONE',  ( 0.000000000000000000, 3.000000000000000000, 0.000000000000000000 ) ) ;
#1280 = AXIS2_PLACEMENT_3D ( 'NONE', #15290, #5359, #5171 ) ;
#1281 = CARTESIAN_POINT ( 'NONE',  ( 4.000000000000000888, -21.59341372045036778, -6.557110696198077626 ) ) ;
#1282 = AXIS2_PLACEMENT_3D ( 'NONE', #15593, #15687, #7048 ) ;
#1283 = CARTESIAN_POINT ( 'NONE',  ( -3.518350579753630747, 38.12180007765648071, -1.080741659609802729 ) ) ;
#1284 = ADVANCED_FACE ( 'NONE', ( #18 ), #3076, .F. ) ;
#1285 = VERTEX_POINT ( 'NONE', #15594 ) ;
#1286 = CARTESIAN_POINT ( 'NONE',  ( 4.000000000000003553, -24.32612312542070754, -14.48614209299050160 ) ) ;
#1287 = ADVANCED_FACE ( 'NONE', ( #14019 ), #108, .T. ) ;
#1288 = CARTESIAN_POINT ( 'NONE',  ( 1.336863392178479160, 16.24680007765647716, -4.297206761780677731 ) ) ;
#1289 = DIRECTION ( 'NONE',  ( -0.000000000000000000, 1.000000000000000000, -0.000000000000000000 ) ) ;
#1290 = CARTESIAN_POINT ( 'NONE',  ( -2.518350579753611207, 39.37819992234354771, 0.7558219633769609480 ) ) ;
#1291 = ORIENTED_EDGE ( 'NONE', *, *, #4095, .F. ) ;
#1292 = CARTESIAN_POINT ( 'NONE',  ( 4.243569643750000786, -25.06175873365810247, -11.51042071350471119 ) ) ;
#1293 = EDGE_CURVE ( 'NONE', #3136, #11085, #11903, .T. ) ;
#1294 = CARTESIAN_POINT ( 'NONE',  ( -4.499999999999999112, 22.99680007765647716, 0.05647727720537927543 ) ) ;
#1295 = ORIENTED_EDGE ( 'NONE', *, *, #5587, .F. ) ;
#1296 = AXIS2_PLACEMENT_3D ( 'NONE', #7926, #9407, #3852 ) ;
#1297 = DIRECTION ( 'NONE',  ( 0.000000000000000000, 0.000000000000000000, -1.000000000000000000 ) ) ;
#1298 = AXIS2_PLACEMENT_3D ( 'NONE', #17832, #10842, #2608 ) ;
#1299 = CARTESIAN_POINT ( 'NONE',  ( -6.428571428571425272, -14.26578344203648285, -2.827263138854410496 ) ) ;
#1300 = CARTESIAN_POINT ( 'NONE',  ( 0.000000000000000000, 15.00000000000000355, 0.000000000000000000 ) ) ;
#1301 = CARTESIAN_POINT ( 'NONE',  ( -4.243569643750000786, -22.86782886461536179, -8.377164144099308984 ) ) ;
#1302 = VERTEX_POINT ( 'NONE', #5762 ) ;
#1303 = LINE ( 'NONE', #15304, #6138 ) ;
#1304 = ORIENTED_EDGE ( 'NONE', *, *, #755, .F. ) ;
#1305 = CARTESIAN_POINT ( 'NONE',  ( 2.000000000000004441, -21.81008232435476657, -12.90602239160557829 ) ) ;
#1306 = CARTESIAN_POINT ( 'NONE',  ( -7.056670106005028309, -10.00000000000000178, -9.351700598554243626 ) ) ;
#1307 = VECTOR ( 'NONE', #10874, 1000.000000000000000 ) ;
#1308 = SURFACE_STYLE_FILL_AREA ( #11111 ) ;
#1309 = FILL_AREA_STYLE_COLOUR ( '', #16948 ) ;
#1310 = CARTESIAN_POINT ( 'NONE',  ( 2.733110507866328920, 18.62819992234354771, 3.862833514489095510 ) ) ;
#1311 = CARTESIAN_POINT ( 'NONE',  ( -2.115076519116425580, 22.37819992234354061, -3.012182706137063182 ) ) ;
#1312 = CARTESIAN_POINT ( 'NONE',  ( 4.000000000000003553, -24.58423252177867369, -14.85476051292054578 ) ) ;
#1313 = CARTESIAN_POINT ( 'NONE',  ( -0.8262555684461330152, 28.49680007765648071, -2.360188852285403982 ) ) ;
#1314 = CARTESIAN_POINT ( 'NONE',  ( -4.499999999999999112, 27.00319992234355126, -0.05647727720528529505 ) ) ;
#1315 = CARTESIAN_POINT ( 'NONE',  ( -4.000000000000000888, -23.72281623969865905, -9.598212659614208775 ) ) ;
#1316 = ORIENTED_EDGE ( 'NONE', *, *, #9101, .F. ) ;
#1317 = CARTESIAN_POINT ( 'NONE',  ( -4.243569643749997233, -17.78508135584820948, -5.389738532321366904 ) ) ;
#1318 = CARTESIAN_POINT ( 'NONE',  ( -3.518350579753630747, 23.12180007765647716, -1.080741659609802729 ) ) ;
#1319 = CARTESIAN_POINT ( 'NONE',  ( 14.20000000000000107, 2.210487472460972698E-16, -1.610000000000000098 ) ) ;
#1320 = CARTESIAN_POINT ( 'NONE',  ( 2.121784821874994176, -25.24372573515406515, -5.363061356521914291 ) ) ;
#1321 = EDGE_CURVE ( 'NONE', #16039, #851, #11329, .T. ) ;
#1322=STYLED_ITEM('',(#18417),#8321);
#1323 = PLANE ( 'NONE',  #6525 ) ;
#1324 = DIRECTION ( 'NONE',  ( 0.000000000000000000, 0.000000000000000000, 1.000000000000000000 ) ) ;
#1325 = CARTESIAN_POINT ( 'NONE',  ( 0.000000000000000000, 43.00000000000000000, 2.500000000000000000 ) ) ;
#1326 = VERTEX_POINT ( 'NONE', #5669 ) ;
#1327 = ORIENTED_EDGE ( 'NONE', *, *, #4949, .T. ) ;
#1328 = CARTESIAN_POINT ( 'NONE',  ( -3.481649420246369697, 22.87180007765647360, 1.193696214020542490 ) ) ;
#1329 = CARTESIAN_POINT ( 'NONE',  ( -4.000000000000000888, -21.91605046519287825, -7.017883720103874623 ) ) ;
#1330 = CARTESIAN_POINT ( 'NONE',  ( -2.000000000000005773, -24.25896670920994680, -4.324438023342780824 ) ) ;
#1331 = CARTESIAN_POINT ( 'NONE',  ( 4.299564228933482956E-15, -23.34993877156982833, -16.03947562923141135 ) ) ;
#1332 = ORIENTED_EDGE ( 'NONE', *, *, #11015, .T. ) ;
#1333 = CARTESIAN_POINT ( 'NONE',  ( 0.05938372350921204690, 37.62819992234354771, -2.628655560595669183 ) ) ;
#1334 = CARTESIAN_POINT ( 'NONE',  ( -4.243569643750000786, -22.57745579371264455, -7.962468421678005726 ) ) ;
#1335 = CARTESIAN_POINT ( 'NONE',  ( 2.115076519116362963, 28.87180007765647716, -3.012182706137107147 ) ) ;
#1336 = CARTESIAN_POINT ( 'NONE',  ( -3.518350579753605434, 26.87819992234354416, 1.080741659609877781 ) ) ;
#1337 = CARTESIAN_POINT ( 'NONE',  ( -1.999999999999996225, -18.41164193897483869, -8.052546529193282510 ) ) ;
#1338 = FACE_OUTER_BOUND ( 'NONE', #14567, .T. ) ;
#1339 = CARTESIAN_POINT ( 'NONE',  ( 2.121784821875004390, -20.97588711224786095, -12.08242646904553474 ) ) ;
#1340 = CARTESIAN_POINT ( 'NONE',  ( -2.237551826324946980, -10.00000000000000178, -12.18738508574780788 ) ) ;
#1341 = LINE ( 'NONE', #16656, #4429 ) ;
#1342 = CYLINDRICAL_SURFACE ( 'NONE', #3202, 2.149999999999995470 ) ;
#1343 = CARTESIAN_POINT ( 'NONE',  ( -2.121784821875005722, -24.25430638244851167, -3.950024080123402559 ) ) ;
#1344 = CARTESIAN_POINT ( 'NONE',  ( -2.013855872281842707, 15.00000000000000533, -2.423565815785008404 ) ) ;
#1345 = CARTESIAN_POINT ( 'NONE',  ( 0.000000000000000000, -27.20729309053124112, -14.57456132866985499 ) ) ;
#1346 = VERTEX_POINT ( 'NONE', #5580 ) ;
#1347 = CARTESIAN_POINT ( 'NONE',  ( 1.593127413382953383, 15.37819992234354594, -2.091722143975172532 ) ) ;
#1348 = EDGE_CURVE ( 'NONE', #13645, #17584, #18248, .T. ) ;
#1349 = CARTESIAN_POINT ( 'NONE',  ( 4.000000000000000888, -23.40017949495614857, -9.137439635708412666 ) ) ;
#1350 = CARTESIAN_POINT ( 'NONE',  ( -3.481649420246370141, 37.87180007765647360, 1.193696214020542268 ) ) ;
#1351 = DIRECTION ( 'NONE',  ( 0.000000000000000000, 1.000000000000000000, 0.000000000000000000 ) ) ;
#1352 = DIRECTION ( 'NONE',  ( 1.000000000000000000, 0.000000000000000000, 0.000000000000000000 ) ) ;
#1353 = ORIENTED_EDGE ( 'NONE', *, *, #13621, .F. ) ;
#1354 = CARTESIAN_POINT ( 'NONE',  ( 4.730628863548789710E-15, -17.62792149424562993, -9.436781100875167638 ) ) ;
#1355 = CARTESIAN_POINT ( 'NONE',  ( -1.135272562821090014, 33.49680007765648071, -3.311245368580554072 ) ) ;
#1356 = SURFACE_STYLE_FILL_AREA ( #14047 ) ;
#1357 = CARTESIAN_POINT ( 'NONE',  ( 4.730628863548789710E-15, -23.01595514321822122, -17.13169061691491279 ) ) ;
#1358 =( BOUNDED_SURFACE ( )  B_SPLINE_SURFACE ( 3, 2, ( 
 ( #8163, #7221, #8517 ),
 ( #15960, #11481, #15767 ),
 ( #3253, #11575, #17175 ),
 ( #11302, #14476, #5929 ),
 ( #285, #1494, #17270 ),
 ( #1587, #4352, #12791 ),
 ( #12877, #4629, #7408 ),
 ( #8892, #10278, #4542 ),
 ( #10184, #10002, #11671 ),
 ( #15861, #3158, #12970 ),
 ( #8795, #1872, #3066 ),
 ( #184, #8605, #14570 ),
 ( #1777, #2885, #12699 ),
 ( #5658, #4449, #15583 ) ),
 .UNSPECIFIED., .F., .F., .F. ) 
 B_SPLINE_SURFACE_WITH_KNOTS ( ( 4, 2, 2, 2, 2, 2, 4 ),
 ( 3, 3 ),
 ( -6.505213034913026604E-18, 0.002393516659216048982, 0.004787033318432104903, 0.007180549977648160824, 0.009574066636864216745, 0.01436109995529632859, 0.01914813327372844043 ),
 ( 0.000000000000000000, 1.000000000000000000 ),
 .UNSPECIFIED. ) 
 GEOMETRIC_REPRESENTATION_ITEM ( )  RATIONAL_B_SPLINE_SURFACE ( (
 ( 1.000000000000000000, 0.5376207706124455088, 1.000000000000000000),
 ( 1.000000000000000000, 0.5651826551449234959, 1.000000000000000000),
 ( 1.000000000000000000, 0.5897230234043094876, 1.000000000000000000),
 ( 1.000000000000000000, 0.6342462738084541085, 1.000000000000000000),
 ( 1.000000000000000000, 0.6542286737548208553, 1.000000000000000000),
 ( 1.000000000000000000, 0.6905470569484681853, 1.000000000000000000),
 ( 1.000000000000000000, 0.7068761916927887023, 1.000000000000000000),
 ( 1.000000000000000000, 0.7364394504874743896, 1.000000000000000000),
 ( 1.000000000000000000, 0.7497141571645004055, 1.000000000000000000),
 ( 1.000000000000000000, 0.7850493443857002873, 1.000000000000000000),
 ( 1.000000000000000000, 0.8026900302402008025, 1.000000000000000000),
 ( 1.000000000000000000, 0.8290821779924412160, 1.000000000000000000),
 ( 1.000000000000000000, 0.8377883503405891830, 1.000000000000000000),
 ( 1.000000000000000000, 0.8431867568967628124, 1.000000000000000000) ) ) 
 REPRESENTATION_ITEM ( '' )  SURFACE ( )  );
#1359 = FACE_OUTER_BOUND ( 'NONE', #10839, .T. ) ;
#1360 = DIRECTION ( 'NONE',  ( 0.000000000000000000, 0.000000000000000000, 1.000000000000000000 ) ) ;
#1361 = CARTESIAN_POINT ( 'NONE',  ( -8.500000000000010658, 14.99364916731036956, 18.34999999999999432 ) ) ;
#1362 = AXIS2_PLACEMENT_3D ( 'NONE', #14070, #1651, #258 ) ;
#1363 = CARTESIAN_POINT ( 'NONE',  ( -5.330712181944245322E-15, -30.39845712766207342, -10.58903566420261910 ) ) ;
#1364 = ORIENTED_EDGE ( 'NONE', *, *, #17337, .T. ) ;
#1365 = CARTESIAN_POINT ( 'NONE',  ( 9.000000000000000000, 16.59999999999999787, -2.500000000000001332 ) ) ;
#1366 = CARTESIAN_POINT ( 'NONE',  ( -5.279047395330986450E-15, -25.69955169211769785, -4.368647641685837968 ) ) ;
#1367 = CARTESIAN_POINT ( 'NONE',  ( 1.135272562821090458, 39.74680007765648071, 3.311245368580554072 ) ) ;
#1368 = ORIENTED_EDGE ( 'NONE', *, *, #5357, .F. ) ;
#1369 = DIRECTION ( 'NONE',  ( -0.000000000000000000, -1.000000000000000000, -0.000000000000000000 ) ) ;
#1370 =( NAMED_UNIT ( * ) SI_UNIT ( $, .STERADIAN. ) SOLID_ANGLE_UNIT ( ) );
#1371 = CARTESIAN_POINT ( 'NONE',  ( -0.05938372350928957516, 16.12180007765647716, -4.731580009072201776 ) ) ;
#1372 = UNCERTAINTY_MEASURE_WITH_UNIT (LENGTH_MEASURE( 1.000000000000000082E-05 ), #11257, 'distance_accuracy_value', 'NONE');
#1373 = CARTESIAN_POINT ( 'NONE',  ( 1.071796769724495224, -20.00604331963507221, -11.26389800479670633 ) ) ;
#1374 = CARTESIAN_POINT ( 'NONE',  ( -2.518350579753611207, 36.87819992234354061, 0.7558219633769609480 ) ) ;
#1375 = AXIS2_PLACEMENT_3D ( 'NONE', #18143, #16652, #18230 ) ;
#1376 = VERTEX_POINT ( 'NONE', #4637 ) ;
#1377 = CARTESIAN_POINT ( 'NONE',  ( 4.243569643750000786, -26.09419631908997772, -12.98489439322490213 ) ) ;
#1378 = CARTESIAN_POINT ( 'NONE',  ( 4.499999999999999112, 34.24680007765646650, -0.05647727720537982360 ) ) ;
#1379 = AXIS2_PLACEMENT_3D ( 'NONE', #16611, #13985, #13803 ) ;
#1380 = ORIENTED_EDGE ( 'NONE', *, *, #7959, .T. ) ;
#1381 = EDGE_CURVE ( 'NONE', #5033, #1782, #14887, .T. ) ;
#1382 = CARTESIAN_POINT ( 'NONE',  ( 0.000000000000000000, 15.00000000000000355, 0.000000000000000000 ) ) ;
#1383 =( LENGTH_UNIT ( ) NAMED_UNIT ( * ) SI_UNIT ( .MILLI., .METRE. ) );
#1384 = ADVANCED_FACE ( 'NONE', ( #11965 ), #2159, .F. ) ;
#1385 = LINE ( 'NONE', #4248, #11708 ) ;
#1386 = PLANE ( 'NONE',  #10932 ) ;
#1387 = CARTESIAN_POINT ( 'NONE',  ( 2.121784821874994176, -26.30842699513068439, -6.883612338733362535 ) ) ;
#1388 = ORIENTED_EDGE ( 'NONE', *, *, #14830, .T. ) ;
#1389 = CARTESIAN_POINT ( 'NONE',  ( -9.000000000000003553, 23.19999999999999574, -2.500000000000001776 ) ) ;
#1390 = ORIENTED_EDGE ( 'NONE', *, *, #6483, .T. ) ;
#1391 = VECTOR ( 'NONE', #1629, 1000.000000000000000 ) ;
#1392 = CARTESIAN_POINT ( 'NONE',  ( -4.000000000000004441, -26.17380387895579830, -9.072267864090346023 ) ) ;
#1393 = FACE_OUTER_BOUND ( 'NONE', #4236, .T. ) ;
#1394 = CARTESIAN_POINT ( 'NONE',  ( 0.000000000000000000, 13.00000000000000178, 2.500000000000000000 ) ) ;
#1395 =( LENGTH_UNIT ( ) NAMED_UNIT ( * ) SI_UNIT ( .MILLI., .METRE. ) );
#1396 = CARTESIAN_POINT ( 'NONE',  ( 4.518350579753602325, 15.62819992234354238, -1.405661355842793725 ) ) ;
#1397 = CARTESIAN_POINT ( 'NONE',  ( -2.211161402132838738, 16.62819992234354416, 2.942372952327218183 ) ) ;
#1398 = CARTESIAN_POINT ( 'NONE',  ( 3.999999999999996447, -28.41075198072487851, -12.26696083681741989 ) ) ;
#1399 = CARTESIAN_POINT ( 'NONE',  ( -1.497042530366477164, 35.12180007765647360, 2.161531897785062384 ) ) ;
#1400 = CARTESIAN_POINT ( 'NONE',  ( -3.607379964056363075, 37.25319992234354061, -2.690724712371229899 ) ) ;
#1401 = CARTESIAN_POINT ( 'NONE',  ( -2.000000000000005773, -26.77553332299520150, -7.918467616653980024 ) ) ;
#1402 = VERTEX_POINT ( 'NONE', #6122 ) ;
#1403 = EDGE_CURVE ( 'NONE', #2406, #9649, #16961, .T. ) ;
#1404 = EDGE_CURVE ( 'NONE', #1787, #196, #16670, .T. ) ;
#1405 = FACE_OUTER_BOUND ( 'NONE', #13425, .T. ) ;
#1406 = ADVANCED_FACE ( 'NONE', ( #7601 ), #11772, .F. ) ;
#1407 = AXIS2_PLACEMENT_3D ( 'NONE', #15441, #6800, #12543 ) ;
#1408 = CARTESIAN_POINT ( 'NONE',  ( 3.518350579753631191, 21.87180007765647360, 1.080741659609802285 ) ) ;
#1409 = CARTESIAN_POINT ( 'NONE',  ( 3.999999999999993339, 0.000000000000000000, 5.000000000000000888 ) ) ;
#1410 = CARTESIAN_POINT ( 'NONE',  ( -2.121784821875005722, -25.80296276059631921, -6.161734599703687643 ) ) ;
#1411 = CARTESIAN_POINT ( 'NONE',  ( -4.518350579753632523, 25.62180007765648426, -1.405661355842698468 ) ) ;
#1412 = CARTESIAN_POINT ( 'NONE',  ( 4.000000000000000888, -22.30321455972984168, -7.570811349998943562 ) ) ;
#1413 = CYLINDRICAL_SURFACE ( 'NONE', #6750, 0.9999999999999991118 ) ;
#1414 = ORIENTED_EDGE ( 'NONE', *, *, #3097, .T. ) ;
#1415 = ORIENTED_EDGE ( 'NONE', *, *, #14028, .F. ) ;
#1416 = SHAPE_REPRESENTATION ( 'socket button head screw_iso_ISO 7380 - M4 x 12 - 12N', ( #16940 ), #8637 ) ;
#1417 = CARTESIAN_POINT ( 'NONE',  ( 3.500000000000000444, 21.74680007765647716, -0.05647727720536935281 ) ) ;
#1418 = DIRECTION ( 'NONE',  ( 3.469446951953612217E-16, -0.000000000000000000, 1.000000000000000000 ) ) ;
#1419 = LINE ( 'NONE', #5668, #14928 ) ;
#1420 = CARTESIAN_POINT ( 'NONE',  ( 4.299564228933482956E-15, -17.73605940148895854, -8.022024996759636650 ) ) ;
#1421 = SURFACE_STYLE_FILL_AREA ( #1505 ) ;
#1422 = ORIENTED_EDGE ( 'NONE', *, *, #16477, .F. ) ;
#1423 = COLOUR_RGB ( '',0.8941176470588234615, 0.8941176470588234615, 0.8941176470588234615 ) ;
#1424 = CARTESIAN_POINT ( 'NONE',  ( 0.05938372350920109732, 17.62819992234354771, -3.680117784833935701 ) ) ;
#1425 = CIRCLE ( 'NONE', #11163, 0.9999999999999991118 ) ;
#1426 = CARTESIAN_POINT ( 'NONE',  ( 4.243569643750000786, -22.70651049189163828, -8.146777631643026041 ) ) ;
#1427 = CARTESIAN_POINT ( 'NONE',  ( -2.518350579753628526, 15.62180007765648071, -0.7558219633769075463 ) ) ;
#1428 = CARTESIAN_POINT ( 'NONE',  ( 2.115076519116426024, 23.62819992234354416, 3.012182706137062294 ) ) ;
#1429 = CARTESIAN_POINT ( 'NONE',  ( -1.071796769724505882, -17.98264209712809958, -8.374181582033761728 ) ) ;
#1430 = DIRECTION ( 'NONE',  ( -0.000000000000000000, -1.000000000000000000, -0.000000000000000000 ) ) ;
#1431 = CARTESIAN_POINT ( 'NONE',  ( 2.121784821874994176, -25.79220820241474854, -6.146375498873266174 ) ) ;
#1432 = CIRCLE ( 'NONE', #11778, 0.9999999999999991118 ) ;
#1433 = CARTESIAN_POINT ( 'NONE',  ( 2.599319604203554679, -24.48737926485759431, -15.99075565718284153 ) ) ;
#1434 = EDGE_CURVE ( 'NONE', #7294, #8864, #1775, .T. ) ;
#1435 = DIRECTION ( 'NONE',  ( -0.000000000000000000, 1.000000000000000000, -0.000000000000000000 ) ) ;
#1436 = FACE_OUTER_BOUND ( 'NONE', #16735, .T. ) ;
#1437 = CARTESIAN_POINT ( 'NONE',  ( -5.330712181944245322E-15, -24.97815980414473103, -2.848048845671618423 ) ) ;
#1438 = CARTESIAN_POINT ( 'NONE',  ( -1.074071013978619593, 15.00000000000066258, -3.257214625843751321 ) ) ;
#1439 = ORIENTED_EDGE ( 'NONE', *, *, #1986, .T. ) ;
#1440 = CARTESIAN_POINT ( 'NONE',  ( -2.518350579753611207, 19.37819992234354771, 0.7558219633769609480 ) ) ;
#1441 = DIRECTION ( 'NONE',  ( -0.000000000000000000, 1.000000000000000000, -0.000000000000000000 ) ) ;
#1442 = CARTESIAN_POINT ( 'NONE',  ( -0.05938372350927861865, 36.12180007765648071, -3.680117784833935701 ) ) ;
#1443 = CONTEXT_DEPENDENT_SHAPE_REPRESENTATION ( #7592, #16708 ) ;
#1444 = PLANE ( 'NONE',  #8387 ) ;
#1445 = DIRECTION ( 'NONE',  ( 1.000000000000000000, 0.000000000000000000, 0.000000000000000000 ) ) ;
#1446 = VERTEX_POINT ( 'NONE', #7416 ) ;
#1447 = CARTESIAN_POINT ( 'NONE',  ( 4.243569643750000786, -20.15768020285669593, -4.506670734833804204 ) ) ;
#1448 = CARTESIAN_POINT ( 'NONE',  ( -2.115076519116362519, 30.12180007765647360, 3.012182706137107147 ) ) ;
#1449 = EDGE_CURVE ( 'NONE', #3078, #1717, #16362, .T. ) ;
#1450 = CARTESIAN_POINT ( 'NONE',  ( -1.734723475976807094E-15, 36.39999999999999147, -2.500000000000000000 ) ) ;
#1451 = CARTESIAN_POINT ( 'NONE',  ( 2.121784821875004390, -22.49227981585092095, -14.24805968613456564 ) ) ;
#1452 = FACE_OUTER_BOUND ( 'NONE', #3465, .T. ) ;
#1453 = EDGE_CURVE ( 'NONE', #14652, #12298, #10116, .T. ) ;
#1454 = AXIS2_PLACEMENT_3D ( 'NONE', #1182, #11165, #2395 ) ;
#1455 = LINE ( 'NONE', #2670, #12411 ) ;
#1456 = CARTESIAN_POINT ( 'NONE',  ( -11.99999999999999822, 13.00000000000000178, -15.00000000000000000 ) ) ;
#1457 = CARTESIAN_POINT ( 'NONE',  ( -2.121784821875005722, -27.35161913874413386, -8.373445119283974947 ) ) ;
#1458 = VERTEX_POINT ( 'NONE', #15872 ) ;
#1459 = CARTESIAN_POINT ( 'NONE',  ( 8.499999999999994671, 15.00000000000000178, 20.49999999999999645 ) ) ;
#1460 = CARTESIAN_POINT ( 'NONE',  ( 1.999999999999994449, -23.18351089105175333, -2.788527940300912444 ) ) ;
#1461 = CARTESIAN_POINT ( 'NONE',  ( -3.500000000000000444, 40.49680007765648071, 0.05647727720536892260 ) ) ;
#1462 = EDGE_LOOP ( 'NONE', ( #3760, #12477, #9504, #5010 ) ) ;
#1463 = CARTESIAN_POINT ( 'NONE',  ( 3.276967058447619152, -25.10900663730464188, -15.57833582608148326 ) ) ;
#1464 = AXIS2_PLACEMENT_3D ( 'NONE', #17122, #15459, #11528 ) ;
#1465 =( LENGTH_UNIT ( ) NAMED_UNIT ( * ) SI_UNIT ( .MILLI., .METRE. ) );
#1466 = DIRECTION ( 'NONE',  ( 1.000000000000000000, 0.000000000000000000, 0.000000000000000000 ) ) ;
#1467 = CARTESIAN_POINT ( 'NONE',  ( -2.055738996568281518, 34.25319992234354061, 1.423772053676066962 ) ) ;
#1468 = ORIENTED_EDGE ( 'NONE', *, *, #10652, .T. ) ;
#1469 = CARTESIAN_POINT ( 'NONE',  ( 4.243569643749997233, -26.57399292614001851, -9.398624849583658403 ) ) ;
#1470 = CIRCLE ( 'NONE', #5021, 0.9999999999999991118 ) ;
#1471 = CARTESIAN_POINT ( 'NONE',  ( -2.733110507866247652, 30.12180007765647716, 3.862833514489154574 ) ) ;
#1472 = ORIENTED_EDGE ( 'NONE', *, *, #17613, .F. ) ;
#1473 = ADVANCED_FACE ( 'NONE', ( #1882 ), #9003, .T. ) ;
#1474 = FACE_OUTER_BOUND ( 'NONE', #8392, .T. ) ;
#1475 = DIRECTION ( 'NONE',  ( -1.000000000000000000, -0.000000000000000000, -0.000000000000000000 ) ) ;
#1476 = CARTESIAN_POINT ( 'NONE',  ( -4.243569643750005227, -23.82082603165501666, -5.466695036996486401 ) ) ;
#1477 = ORIENTED_EDGE ( 'NONE', *, *, #3659, .F. ) ;
#1478 = LINE ( 'NONE', #2958, #7925 ) ;
#1479 = ORIENTED_EDGE ( 'NONE', *, *, #10509, .F. ) ;
#1480 = EDGE_LOOP ( 'NONE', ( #17026, #9744, #18292, #16872 ) ) ;
#1481 = DIRECTION ( 'NONE',  ( -4.915049848600951133E-16, 0.000000000000000000, -1.000000000000000000 ) ) ;
#1482 = FACE_OUTER_BOUND ( 'NONE', #12182, .T. ) ;
#1483 =( LENGTH_UNIT ( ) NAMED_UNIT ( * ) SI_UNIT ( .MILLI., .METRE. ) );
#1484 = CARTESIAN_POINT ( 'NONE',  ( -1.444289557195956863, 21.50319992234354771, 4.262301884875733471 ) ) ;
#1485 = CARTESIAN_POINT ( 'NONE',  ( -2.864755990943222308, 29.25319992234354416, 2.011557305968548093 ) ) ;
#1486 = CARTESIAN_POINT ( 'NONE',  ( -1.999999999999996225, -23.83193926249218109, -15.79353334772428497 ) ) ;
#1487 = CARTESIAN_POINT ( 'NONE',  ( -2.055738996568313048, 38.24680007765647360, -1.423772053676023441 ) ) ;
#1488 = CARTESIAN_POINT ( 'NONE',  ( 0.05938372350919016857, 35.12819992234354771, -4.731580009072201776 ) ) ;
#1489 = CARTESIAN_POINT ( 'NONE',  ( -1.999999999999996225, -20.92820855276008629, -11.64657612250448437 ) ) ;
#1490 = ORIENTED_EDGE ( 'NONE', *, *, #1047, .F. ) ;
#1491 = CIRCLE ( 'NONE', #5911, 0.9999999999999991118 ) ;
#1492 = FACE_OUTER_BOUND ( 'NONE', #1480, .T. ) ;
#1493 = CARTESIAN_POINT ( 'NONE',  ( -3.518350579753630747, 20.62180007765646650, -1.080741659609802729 ) ) ;
#1494 = CARTESIAN_POINT ( 'NONE',  ( -6.270298154903644949, -10.34439663368850937, 0.7558933527348972170 ) ) ;
#1495 = CARTESIAN_POINT ( 'NONE',  ( 2.121784821875004390, -19.65307645591326846, -10.19325706690404054 ) ) ;
#1496 = CARTESIAN_POINT ( 'NONE',  ( 4.518350579753633411, 24.37180007765647005, 1.405661355842698468 ) ) ;
#1497 = CARTESIAN_POINT ( 'NONE',  ( -1.071796769724496334, -23.13931017290888903, -1.791092450922006529 ) ) ;
#1498 = DIRECTION ( 'NONE',  ( 1.000000000000000000, 0.000000000000000000, -4.336808689942021680E-16 ) ) ;
#1499 = EDGE_LOOP ( 'NONE', ( #16781, #12095, #7487, #14745 ) ) ;
#1500 = VERTEX_POINT ( 'NONE', #13446 ) ;
#1501 = CARTESIAN_POINT ( 'NONE',  ( -3.500000000000000444, 25.49680007765647716, 0.05647727720536892260 ) ) ;
#1502 = CARTESIAN_POINT ( 'NONE',  ( -2.000000000000005773, -26.00120513392129240, -6.812612356863837704 ) ) ;
#1503 = EDGE_CURVE ( 'NONE', #4478, #6078, #16156, .T. ) ;
#1504 = CARTESIAN_POINT ( 'NONE',  ( 9.999999999999998224, 27.59999999999999432, -2.500000000000001776 ) ) ;
#1505 = FILL_AREA_STYLE ('',( #15333 ) ) ;
#1506 = ORIENTED_EDGE ( 'NONE', *, *, #18083, .T. ) ;
#1507 = AXIS2_PLACEMENT_3D ( 'NONE', #2357, #6777, #8078 ) ;
#1508 = CARTESIAN_POINT ( 'NONE',  ( 3.481649420246394122, 20.87819992234354416, 1.193696214020467439 ) ) ;
#1509 = ADVANCED_FACE ( 'NONE', ( #760, #4919 ), #10384, .F. ) ;
#1510 = CARTESIAN_POINT ( 'NONE',  ( -2.121784821875005722, -25.54485336423835307, -5.793116179773641683 ) ) ;
#1511 = CARTESIAN_POINT ( 'NONE',  ( -0.7188294034286043521, 17.49680007765647716, 2.395093729190366005 ) ) ;
#1512 = EDGE_CURVE ( 'NONE', #5839, #5725, #15475, .T. ) ;
#1513 = CARTESIAN_POINT ( 'NONE',  ( -2.115076519116425580, 32.37819992234354771, -3.012182706137062738 ) ) ;
#1514 = CARTESIAN_POINT ( 'NONE',  ( 1.300000000000000044, 1.443375672974065216, 7.222237291452134449E-31 ) ) ;
#1515 = CARTESIAN_POINT ( 'NONE',  ( 3.999999999999996447, -26.86209560257706030, -10.05525031723713347 ) ) ;
#1516 = EDGE_CURVE ( 'NONE', #8485, #2986, #3660, .T. ) ;
#1517 = CARTESIAN_POINT ( 'NONE',  ( 4.243569643749996345, -23.99289896256033572, -5.712440650283179266 ) ) ;
#1518 = CIRCLE ( 'NONE', #1814, 0.9999999999999991118 ) ;
#1519 =( BOUNDED_CURVE ( )  B_SPLINE_CURVE ( 3, ( #14527, #7181, #8944, #5886 ),
 .UNSPECIFIED., .F., .F. ) 
 B_SPLINE_CURVE_WITH_KNOTS ( ( 4, 4 ),
 ( 0.000000000000000000, 1.029696800837752058 ),
 .UNSPECIFIED. ) 
 CURVE ( )  GEOMETRIC_REPRESENTATION_ITEM ( )  RATIONAL_B_SPLINE_CURVE ( ( 1.000000000000000000, 0.9135782535825734962, 0.9135782535825734962, 1.000000000000000000 ) ) 
 REPRESENTATION_ITEM ( '' )  );
#1520 = EDGE_CURVE ( 'NONE', #6047, #10458, #5547, .T. ) ;
#1521 = CARTESIAN_POINT ( 'NONE',  ( -8.511038526056534437, -10.00000000000000178, -5.033916384140056266 ) ) ;
#1522 = CARTESIAN_POINT ( 'NONE',  ( -1.734723475976807094E-15, 31.99999999999999289, -11.50000000000000178 ) ) ;
#1523 = CARTESIAN_POINT ( 'NONE',  ( -14.99999999999999645, 10.00000000000000000, 30.00000000000000000 ) ) ;
#1524 = CARTESIAN_POINT ( 'NONE',  ( 2.121784821875004390, -17.58820128504952152, -7.244309707463659542 ) ) ;
#1525 = LINE ( 'NONE', #7342, #6209 ) ;
#1526 = FACE_OUTER_BOUND ( 'NONE', #6394, .T. ) ;
#1527 = EDGE_LOOP ( 'NONE', ( #16504, #13644, #6239, #8457 ) ) ;
#1528 = CARTESIAN_POINT ( 'NONE',  ( -0.8262555684460826111, 16.50319992234354416, 2.360188852285421302 ) ) ;
#1529 = CARTESIAN_POINT ( 'NONE',  ( 2.121784821874994176, -29.63158547323952874, -11.62957449533272580 ) ) ;
#1530 = CARTESIAN_POINT ( 'NONE',  ( 2.115076519116362963, 18.87180007765648071, -3.012182706137107147 ) ) ;
#1531 = AXIS2_PLACEMENT_3D ( 'NONE', #4749, #17198, #10301 ) ;
#1532 = FACE_OUTER_BOUND ( 'NONE', #7483, .T. ) ;
#1533 = FACE_BOUND ( 'NONE', #8591, .T. ) ;
#1534 = ORIENTED_EDGE ( 'NONE', *, *, #210, .T. ) ;
#1535 = CARTESIAN_POINT ( 'NONE',  ( 2.121784821874994176, -23.21111423883506220, -2.460191299572788814 ) ) ;
#1536 = CARTESIAN_POINT ( 'NONE',  ( 1.135272562821090458, 29.74680007765647716, 3.311245368580554072 ) ) ;
#1537 = CARTESIAN_POINT ( 'NONE',  ( 4.243569643749996345, -28.89697749336173871, -12.71619062895408803 ) ) ;
#1538 = FACE_OUTER_BOUND ( 'NONE', #12873, .T. ) ;
#1539 = CARTESIAN_POINT ( 'NONE',  ( 4.730628863548789710E-15, -21.98351755778634953, -15.65721693719472185 ) ) ;
#1540 = DIRECTION ( 'NONE',  ( 0.000000000000000000, 0.000000000000000000, -1.000000000000000000 ) ) ;
#1541 =( GEOMETRIC_REPRESENTATION_CONTEXT ( 3 ) GLOBAL_UNCERTAINTY_ASSIGNED_CONTEXT ( ( #5473 ) ) GLOBAL_UNIT_ASSIGNED_CONTEXT ( ( #13339, #1764, #272 ) ) REPRESENTATION_CONTEXT ( 'NONE', 'WORKASPACE' ) );
#1542 = CARTESIAN_POINT ( 'NONE',  ( -1.661723472263481630E-14, -21.34959095050052014, -13.18268287578030318 ) ) ;
#1543 = DIRECTION ( 'NONE',  ( 0.000000000000000000, 0.000000000000000000, 1.000000000000000000 ) ) ;
#1544 = CARTESIAN_POINT ( 'NONE',  ( -4.243569643750005227, -26.11154692433198576, -8.738183513875661390 ) ) ;
#1545 = DIRECTION ( 'NONE',  ( -0.000000000000000000, -0.5735764363510414965, -0.8191520442889950182 ) ) ;
#1546 = CARTESIAN_POINT ( 'NONE',  ( 4.000000000000003553, -18.38960700918742575, -6.007918434599401891 ) ) ;
#1547 = CARTESIAN_POINT ( 'NONE',  ( -1.593127413382998459, 20.87180007765648426, -2.091722143975139669 ) ) ;
#1548 = VERTEX_POINT ( 'NONE', #2430 ) ;
#1549 = CARTESIAN_POINT ( 'NONE',  ( 3.500000000000000444, 21.74680007765647716, -0.05647727720536935281 ) ) ;
#1550 = AXIS2_PLACEMENT_3D ( 'NONE', #5822, #8419, #10170 ) ;
#1551 = FACE_OUTER_BOUND ( 'NONE', #4692, .T. ) ;
#1552 = CARTESIAN_POINT ( 'NONE',  ( 0.8262555684460829442, 32.75319992234354061, -2.360188852285421302 ) ) ;
#1553 = MANIFOLD_SOLID_BREP ( 'LPattern6[5]', #11416 ) ;
#1554 = ORIENTED_EDGE ( 'NONE', *, *, #5294, .F. ) ;
#1555 = CARTESIAN_POINT ( 'NONE',  ( -2.121784821874996396, -20.67475948316355883, -11.65237164579381535 ) ) ;
#1556 = PRODUCT_DEFINITION_FORMATION_WITH_SPECIFIED_SOURCE ( 'ANY', '', #17623, .NOT_KNOWN. ) ;
#1557 = CARTESIAN_POINT ( 'NONE',  ( -2.829195390882805139, 30.87180007765647716, -3.793023760679206102 ) ) ;
#1558 = ORIENTED_EDGE ( 'NONE', *, *, #10050, .T. ) ;
#1559 =( NAMED_UNIT ( * ) SI_UNIT ( $, .STERADIAN. ) SOLID_ANGLE_UNIT ( ) );
#1560 = DIRECTION ( 'NONE',  ( 0.000000000000000000, 0.000000000000000000, -1.000000000000000000 ) ) ;
#1561 = CARTESIAN_POINT ( 'NONE',  ( 9.000000000000000000, 29.79999999999999716, -2.500000000000001332 ) ) ;
#1562 = VECTOR ( 'NONE', #1193, 1000.000000000000000 ) ;
#1563 = CARTESIAN_POINT ( 'NONE',  ( -1.999999999999996225, -23.05761107341827199, -14.68767808793413998 ) ) ;
#1564 = CIRCLE ( 'NONE', #16681, 2.149999999999999023 ) ;
#1565 = CARTESIAN_POINT ( 'NONE',  ( -8.000000000000003553, 38.59999999999999432, -2.500000000000001776 ) ) ;
#1566 = CARTESIAN_POINT ( 'NONE',  ( -2.121784821874996396, -18.09366551958387248, -7.966187446493337987 ) ) ;
#1567 = VERTEX_POINT ( 'NONE', #15310 ) ;
#1568 = CARTESIAN_POINT ( 'NONE',  ( -4.518350579753602325, 16.87819992234354416, 1.405661355842794391 ) ) ;
#1569 = FACE_OUTER_BOUND ( 'NONE', #11023, .T. ) ;
#1570 = ORIENTED_EDGE ( 'NONE', *, *, #1434, .T. ) ;
#1571 = ORIENTED_EDGE ( 'NONE', *, *, #3061, .F. ) ;
#1572 = PLANE ( 'NONE',  #2737 ) ;
#1573 = DIRECTION ( 'NONE',  ( -1.000000000000000000, -0.000000000000000000, -0.000000000000000000 ) ) ;
#1574 = CARTESIAN_POINT ( 'NONE',  ( -4.499999999999999112, 19.50319992234354416, -0.05647727720528529505 ) ) ;
#1575 = CARTESIAN_POINT ( 'NONE',  ( 2.798362969681409851, 28.50319992234354416, 2.102939460078764977 ) ) ;
#1576 = EDGE_CURVE ( 'NONE', #17808, #9317, #9237, .T. ) ;
#1577 = CARTESIAN_POINT ( 'NONE',  ( -0.8262555684461330152, 35.99680007765648071, -2.360188852285403982 ) ) ;
#1578 = AXIS2_PLACEMENT_3D ( 'NONE', #14959, #10574, #16159 ) ;
#1579 = VERTEX_POINT ( 'NONE', #5191 ) ;
#1580 = CARTESIAN_POINT ( 'NONE',  ( 4.481649420246397675, 35.87819992234354771, 1.518615910253363177 ) ) ;
#1581 = CIRCLE ( 'NONE', #11934, 0.9999999999999991118 ) ;
#1582 = CARTESIAN_POINT ( 'NONE',  ( 4.713407268011036227E-15, -19.22951417349437619, -11.23374808423137949 ) ) ;
#1583 = ORIENTED_EDGE ( 'NONE', *, *, #1403, .T. ) ;
#1584 = CARTESIAN_POINT ( 'NONE',  ( 0.000000000000000000, 5.977523610840987267, 32.81826849749789687 ) ) ;
#1585 = CARTESIAN_POINT ( 'NONE',  ( 2.115076519116362963, 26.37180007765648071, -3.012182706137107147 ) ) ;
#1586 = MANIFOLD_SOLID_BREP ( 'Boss-Extrude2', #14466 ) ;
#1587 = CARTESIAN_POINT ( 'NONE',  ( -9.829077985114366811, -9.943001520064436605, 1.739096673092067613 ) ) ;
#1588 = CARTESIAN_POINT ( 'NONE',  ( 4.730628863548789710E-15, -18.36998600877478793, -10.49655905817405355 ) ) ;
#1589 = CARTESIAN_POINT ( 'NONE',  ( -0.05938372350928957516, 33.62180007765647360, -4.731580009072201776 ) ) ;
#1590 = VECTOR ( 'NONE', #3105, 1000.000000000000000 ) ;
#1591 = VERTEX_POINT ( 'NONE', #11027 ) ;
#1592 = ORIENTED_EDGE ( 'NONE', *, *, #16531, .F. ) ;
#1593 = CARTESIAN_POINT ( 'NONE',  ( 1.135272562821090458, 27.24680007765648071, 3.311245368580554072 ) ) ;
#1594 = CARTESIAN_POINT ( 'NONE',  ( 4.299564228933482956E-15, -19.99451661891623289, -11.24743617014079078 ) ) ;
#1595 =( NAMED_UNIT ( * ) PLANE_ANGLE_UNIT ( ) SI_UNIT ( $, .RADIAN. ) );
#1596 = CARTESIAN_POINT ( 'NONE',  ( -1.999999999999996225, -18.66975133533280484, -8.421164949123328469 ) ) ;
#1597 = ORIENTED_EDGE ( 'NONE', *, *, #4750, .T. ) ;
#1598 = CARTESIAN_POINT ( 'NONE',  ( -2.115076519116425580, 19.87819992234354416, -3.012182706137062738 ) ) ;
#1599 = CARTESIAN_POINT ( 'NONE',  ( 4.243569643749996345, -24.21874468437355432, -6.034981767721971480 ) ) ;
#1600 = CARTESIAN_POINT ( 'NONE',  ( -2.211161402132902243, 38.37180007765648071, -2.942372952327172886 ) ) ;
#1601 = CARTESIAN_POINT ( 'NONE',  ( -2.211161402132839182, 31.62819992234354416, 2.942372952327218627 ) ) ;
#1602 = DIRECTION ( 'NONE',  ( -0.000000000000000000, 1.000000000000000000, -0.000000000000000000 ) ) ;
#1603 = DIRECTION ( 'NONE',  ( -1.000000000000000000, -0.000000000000000000, -0.000000000000000000 ) ) ;
#1604 = CONICAL_SURFACE ( 'NONE', #12245, 1.610000000000000098, 0.7853981633974469467 ) ;
#1605 = CARTESIAN_POINT ( 'NONE',  ( -4.243569643749997233, -21.14050350850180138, -10.18177799141198747 ) ) ;
#1606 = DIRECTION ( 'NONE',  ( -0.000000000000000000, -0.5735764363510414965, -0.8191520442889950182 ) ) ;
#1607 = EDGE_CURVE ( 'NONE', #7588, #10009, #9632, .T. ) ;
#1608 = ADVANCED_FACE ( 'NONE', ( #1216 ), #3033, .T. ) ;
#1609 = CARTESIAN_POINT ( 'NONE',  ( -3.973088838427990765, -15.08697326462699095, -8.369503528064965892 ) ) ;
#1610 = DIRECTION ( 'NONE',  ( -1.000000000000000000, 0.000000000000000000, 0.000000000000000000 ) ) ;
#1611 = CARTESIAN_POINT ( 'NONE',  ( -4.000000000000004441, -26.62549532187730250, -9.717350097961160671 ) ) ;
#1612 = CARTESIAN_POINT ( 'NONE',  ( 2.121784821875004390, -17.33009188869154826, -6.875691287533610918 ) ) ;
#1613 = DIRECTION ( 'NONE',  ( 0.000000000000000000, 0.5150380737757255245, 0.8571673013836856869 ) ) ;
#1614 = CYLINDRICAL_SURFACE ( 'NONE', #16233, 2.499999999999999556 ) ;
#1615 = ORIENTED_EDGE ( 'NONE', *, *, #2991, .F. ) ;
#1616 = CARTESIAN_POINT ( 'NONE',  ( 1.989345975306457071, 18.50319992234354416, 1.515154207786300500 ) ) ;
#1617 = CARTESIAN_POINT ( 'NONE',  ( -4.243569643750005227, -28.69264088791166856, -12.42436771317613875 ) ) ;
#1618 = DIRECTION ( 'NONE',  ( 0.000000000000000000, 0.000000000000000000, 1.000000000000000000 ) ) ;
#1619 = LINE ( 'NONE', #15536, #1590 ) ;
#1620 = CARTESIAN_POINT ( 'NONE',  ( 6.428571428571432378, -14.26578344203647930, -2.827263138854372748 ) ) ;
#1621 = ORIENTED_EDGE ( 'NONE', *, *, #7906, .T. ) ;
#1622 = CARTESIAN_POINT ( 'NONE',  ( 4.243569643749997233, -22.18613318805455847, -3.132111710772846891 ) ) ;
#1623 = CARTESIAN_POINT ( 'NONE',  ( 2.115076519116362963, 36.37180007765648782, -3.012182706137107147 ) ) ;
#1624 = CARTESIAN_POINT ( 'NONE',  ( 4.243569643750003451, -25.09818091932399398, -15.83392709700605039 ) ) ;
#1625 =( BOUNDED_CURVE ( )  B_SPLINE_CURVE ( 2, ( #4738, #13167, #10097, #5937, #11680, #4638, #6123, #10289, #11587 ),
 .UNSPECIFIED., .F., .T. ) 
 B_SPLINE_CURVE_WITH_KNOTS ( ( 3, 2, 2, 2, 3 ),
 ( 0.07758620689655172653, 0.08045977011494252762, 0.08620689655172414367, 0.09195402298850574585, 0.09482758620689656082 ),
 .UNSPECIFIED. ) 
 CURVE ( )  GEOMETRIC_REPRESENTATION_ITEM ( )  RATIONAL_B_SPLINE_CURVE ( ( 0.9330127018922194093, 0.9330127018922194093, 1.000000000000000000, 0.8660254037844387076, 1.000000000000000000, 0.8660254037844387076, 1.000000000000000000, 0.9330127018922191873, 0.9330127018922194093 ) ) 
 REPRESENTATION_ITEM ( '' )  );
#1626 = EDGE_CURVE ( 'NONE', #13968, #11829, #7434, .T. ) ;
#1627 = EDGE_CURVE ( 'NONE', #14839, #14660, #13202, .T. ) ;
#1628 = CARTESIAN_POINT ( 'NONE',  ( 2.121784821875004390, -23.26660800492483006, -15.35391494592470885 ) ) ;
#1629 = DIRECTION ( 'NONE',  ( -0.000000000000000000, -0.5735764363510414965, -0.8191520442889950182 ) ) ;
#1630 = CARTESIAN_POINT ( 'NONE',  ( -3.999999999999997335, -22.69143028182022803, -12.15155876676686830 ) ) ;
#1631 = DIRECTION ( 'NONE',  ( 0.000000000000000000, 0.000000000000000000, -1.000000000000000000 ) ) ;
#1632 = CARTESIAN_POINT ( 'NONE',  ( -2.121784821875005722, -27.60972853510210001, -8.742063539214022683 ) ) ;
#1633 = CARTESIAN_POINT ( 'NONE',  ( -5.577813053751546416E-15, -28.74166284227092305, -9.792081248737861898 ) ) ;
#1634 = CARTESIAN_POINT ( 'NONE',  ( -5.279047395330986450E-15, -24.66711410668581550, -2.894173961965647912 ) ) ;
#1635 = CARTESIAN_POINT ( 'NONE',  ( 0.05938372350926800214, 19.87180007765648426, 2.628655560595669183 ) ) ;
#1636 = ORIENTED_EDGE ( 'NONE', *, *, #15905, .T. ) ;
#1637 = CARTESIAN_POINT ( 'NONE',  ( -2.864755990943265829, 25.74680007765647716, -2.011557305968488141 ) ) ;
#1638 = DIRECTION ( 'NONE',  ( 0.000000000000000000, 0.000000000000000000, 1.000000000000000000 ) ) ;
#1639 = DIRECTION ( 'NONE',  ( 1.000000000000000000, 0.000000000000000000, 0.000000000000000000 ) ) ;
#1640 = CARTESIAN_POINT ( 'NONE',  ( 4.299564228933482956E-15, -19.99451661891623289, -11.24743617014079078 ) ) ;
#1641 = CARTESIAN_POINT ( 'NONE',  ( -1.593127413382952939, 34.12819992234354771, 2.091722143975172532 ) ) ;
#1642 = MANIFOLD_SOLID_BREP ( 'Hex', #18027 ) ;
#1643 = EDGE_LOOP ( 'NONE', ( #15088, #14719, #5176 ) ) ;
#1644 = CARTESIAN_POINT ( 'NONE',  ( -5.330712181944246111E-15, -28.36584563134307047, -7.686165607253494514 ) ) ;
#1645 = CARTESIAN_POINT ( 'NONE',  ( 3.607379964056306676, 36.49680007765646650, -2.690724712371305838 ) ) ;
#1646 = ORIENTED_EDGE ( 'NONE', *, *, #1172, .F. ) ;
#1647 = AXIS2_PLACEMENT_3D ( 'NONE', #18229, #12539, #25 ) ;
#1648 = FACE_OUTER_BOUND ( 'NONE', #6847, .T. ) ;
#1649 = CARTESIAN_POINT ( 'NONE',  ( 4.000000000000000888, -22.81943335244577398, -8.308048189859038146 ) ) ;
#1650 = CARTESIAN_POINT ( 'NONE',  ( 2.121784821874994176, -28.11519276963646519, -9.463941278243694910 ) ) ;
#1651 = DIRECTION ( 'NONE',  ( -0.000000000000000000, 1.000000000000000000, -0.000000000000000000 ) ) ;
#1652 = DIRECTION ( 'NONE',  ( 0.000000000000000000, 0.000000000000000000, -1.000000000000000000 ) ) ;
#1653 = DIRECTION ( 'NONE',  ( 3.469446951953612217E-16, -0.000000000000000000, 1.000000000000000000 ) ) ;
#1654 = CARTESIAN_POINT ( 'NONE',  ( 4.243569643750003451, -19.67788359580665869, -8.092940278475046156 ) ) ;
#1655 = ORIENTED_EDGE ( 'NONE', *, *, #16460, .T. ) ;
#1656 = CARTESIAN_POINT ( 'NONE',  ( 0.000000000000000000, 9.254131787996968228, 30.52396275209373044 ) ) ;
#1657 = ORIENTED_EDGE ( 'NONE', *, *, #3378, .T. ) ;
#1658 = ORIENTED_EDGE ( 'NONE', *, *, #2419, .T. ) ;
#1659 = AXIS2_PLACEMENT_3D ( 'NONE', #14303, #16924, #205 ) ;
#1660 = CARTESIAN_POINT ( 'NONE',  ( -1.071796769724486786, -17.20831390805418337, -7.268326322243626514 ) ) ;
#1661 = LINE ( 'NONE', #13148, #1870 ) ;
#1662 = PRODUCT_CONTEXT ( 'NONE', #15786, 'mechanical' ) ;
#1663 = CARTESIAN_POINT ( 'NONE',  ( -4.499999999999999112, 14.50319992234354594, -0.05647727720528529505 ) ) ;
#1664 = CARTESIAN_POINT ( 'NONE',  ( 3.500000000000000444, 25.75319992234354771, 0.05647727720529520379 ) ) ;
#1665 = AXIS2_PLACEMENT_3D ( 'NONE', #17115, #2921, #11522 ) ;
#1666 = CARTESIAN_POINT ( 'NONE',  ( -2.500000000000001332, 14.50319992234354771, -0.05647727720530596601 ) ) ;
#1667 = VERTEX_POINT ( 'NONE', #15754 ) ;
#1668 = CARTESIAN_POINT ( 'NONE',  ( 3.673772985318163098, 35.50319992234354771, -2.599342558261029001 ) ) ;
#1669 = ADVANCED_FACE ( 'NONE', ( #8685 ), #18281, .F. ) ;
#1670 = CARTESIAN_POINT ( 'NONE',  ( -5.279047395330986450E-15, -27.18368072047107020, -6.488203555276846224 ) ) ;
#1671 = VERTEX_POINT ( 'NONE', #4813 ) ;
#1672 = EDGE_CURVE ( 'NONE', #11075, #3556, #12208, .T. ) ;
#1673 = DIRECTION ( 'NONE',  ( -1.000000000000000000, 0.000000000000000000, 0.000000000000000000 ) ) ;
#1674 = CARTESIAN_POINT ( 'NONE',  ( -1.135272562821090014, 33.49680007765648071, -3.311245368580554072 ) ) ;
#1675 = ADVANCED_FACE ( 'NONE', ( #8333 ), #9249, .T. ) ;
#1676 = CARTESIAN_POINT ( 'NONE',  ( 2.121784821874994176, -24.21128814972218990, -3.888587676801722903 ) ) ;
#1677 = EDGE_CURVE ( 'NONE', #13721, #297, #14916, .T. ) ;
#1678 = VECTOR ( 'NONE', #12083, 1000.000000000000000 ) ;
#1679 = CARTESIAN_POINT ( 'NONE',  ( -4.481649420246366589, 30.37180007765647716, 1.518615910253458878 ) ) ;
#1680 = CARTESIAN_POINT ( 'NONE',  ( -9.000000000000001776, 36.39999999999999147, 2.499999999999998224 ) ) ;
#1681 = VERTEX_POINT ( 'NONE', #4169 ) ;
#1682 = VERTEX_POINT ( 'NONE', #16980 ) ;
#1683 = CARTESIAN_POINT ( 'NONE',  ( 2.864755990943265829, 21.99680007765647716, 2.011557305968487697 ) ) ;
#1684 = DIRECTION ( 'NONE',  ( -0.000000000000000000, -0.000000000000000000, 1.000000000000000000 ) ) ;
#1685 = CARTESIAN_POINT ( 'NONE',  ( -2.000000000000005773, -28.90493584365338720, -10.95956958208364007 ) ) ;
#1686 = DIRECTION ( 'NONE',  ( 0.000000000000000000, 0.000000000000000000, -1.000000000000000000 ) ) ;
#1687 = SURFACE_SIDE_STYLE ('',( #8710 ) ) ;
#1688 = EDGE_LOOP ( 'NONE', ( #4787, #12072, #16035, #6829 ) ) ;
#1689 = CARTESIAN_POINT ( 'NONE',  ( 2.864755990943222308, 18.00319992234354771, -2.011557305968548093 ) ) ;
#1690 = CYLINDRICAL_SURFACE ( 'NONE', #91, 2.000000000000000000 ) ;
#1691 = CARTESIAN_POINT ( 'NONE',  ( -2.121784821874996396, -19.86816761954490573, -10.50043908351241662 ) ) ;
#1692 = CARTESIAN_POINT ( 'NONE',  ( 1.593127413382998903, 17.12180007765648426, 2.091722143975139669 ) ) ;
#1693 = CLOSED_SHELL ( 'NONE', ( #4887, #6609, #18089, #13508, #4115, #17290, #2052, #11859, #3622, #7740 ) ) ;
#1694 = CARTESIAN_POINT ( 'NONE',  ( 2.115076519116426024, 33.62819992234353350, 3.012182706137062294 ) ) ;
#1695 = CARTESIAN_POINT ( 'NONE',  ( -2.121784821874996396, -23.51396284310121487, -15.70717426502434044 ) ) ;
#1696 = AXIS2_PLACEMENT_3D ( 'NONE', #10677, #16349, #958 ) ;
#1697 = CARTESIAN_POINT ( 'NONE',  ( -3.999999999999997335, -25.20799689560547918, -15.74558836007806839 ) ) ;
#1698 = CARTESIAN_POINT ( 'NONE',  ( -4.243569643750005227, -24.85326361708688836, -6.941168716716678233 ) ) ;
#1699 = DIRECTION ( 'NONE',  ( 0.000000000000000000, 0.8191520442889952403, -0.5735764363510413855 ) ) ;
#1700 = EDGE_CURVE ( 'NONE', #8879, #3333, #8420, .T. ) ;
#1701 = EDGE_CURVE ( 'NONE', #8991, #2259, #3048, .T. ) ;
#1702 = CARTESIAN_POINT ( 'NONE',  ( -2.220605816132459776, -15.34963770581800624, -10.14223552587114874 ) ) ;
#1703 = CARTESIAN_POINT ( 'NONE',  ( 0.000000000000000000, 43.00000000000000000, 2.500000000000000000 ) ) ;
#1704 = AXIS2_PLACEMENT_3D ( 'NONE', #1389, #18104, #3890 ) ;
#1705 = FACE_OUTER_BOUND ( 'NONE', #17283, .T. ) ;
#1706 = TOROIDAL_SURFACE ( 'NONE', #12936, 9.000000000000001776, 0.9999999999999991118 ) ;
#1707 = CARTESIAN_POINT ( 'NONE',  ( 4.243569643750003451, -18.09696354311409294, -5.835152456403505106 ) ) ;
#1708 = CARTESIAN_POINT ( 'NONE',  ( 2.000000000000004441, -21.81008232435476657, -12.90602239160557829 ) ) ;
#1709 = CARTESIAN_POINT ( 'NONE',  ( 4.299564228933482956E-15, -19.47829782620029704, -10.51019933028069708 ) ) ;
#1710 = ORIENTED_EDGE ( 'NONE', *, *, #12163, .F. ) ;
#1711 = CARTESIAN_POINT ( 'NONE',  ( -2.055738996568281518, 16.75319992234354416, 1.423772053676066962 ) ) ;
#1712 = CARTESIAN_POINT ( 'NONE',  ( -5.330712181944245322E-15, -30.39845712766207342, -10.58903566420261910 ) ) ;
#1713 = DIRECTION ( 'NONE',  ( -3.373073425510457965E-16, 0.000000000000000000, -1.000000000000000000 ) ) ;
#1714 = CARTESIAN_POINT ( 'NONE',  ( -4.518350579753632523, 15.62180007765647360, -1.405661355842698468 ) ) ;
#1715 = DIRECTION ( 'NONE',  ( -1.000000000000000000, 0.000000000000000000, 0.000000000000000000 ) ) ;
#1716 = CARTESIAN_POINT ( 'NONE',  ( 4.193264170086575149, -10.00000000000000533, -2.677076674082570218 ) ) ;
#1717 = VERTEX_POINT ( 'NONE', #8503 ) ;
#1718 = CARTESIAN_POINT ( 'NONE',  ( 2.121784821874994176, -22.95300484247709250, -2.091572879642740634 ) ) ;
#1719 = CARTESIAN_POINT ( 'NONE',  ( 3.500000000000000444, 36.74680007765648071, -0.05647727720536935281 ) ) ;
#1720 = AXIS2_PLACEMENT_3D ( 'NONE', #7114, #5912, #15845 ) ;
#1721 = CARTESIAN_POINT ( 'NONE',  ( -4.243569643750005227, -28.72490456245641965, -12.47044501566739427 ) ) ;
#1722 = AXIS2_PLACEMENT_3D ( 'NONE', #17321, #4585, #17511 ) ;
#1723 = CARTESIAN_POINT ( 'NONE',  ( -1.999999999999996225, -22.28328288434436644, -13.58182282814399855 ) ) ;
#1724 = CARTESIAN_POINT ( 'NONE',  ( -4.243569643749998122, -23.94744319389470988, -14.19050330815125704 ) ) ;
#1725 = CARTESIAN_POINT ( 'NONE',  ( 1.999999999999994449, -22.60276474854137874, -1.959136494451539035 ) ) ;
#1726 = DIRECTION ( 'NONE',  ( 0.000000000000000000, -0.000000000000000000, 1.000000000000000000 ) ) ;
#1727 = LINE ( 'NONE', #7361, #2899 ) ;
#1728 = CARTESIAN_POINT ( 'NONE',  ( 4.730628863548789710E-15, -20.17675178328056873, -13.07688799768438948 ) ) ;
#1729 = DIRECTION ( 'NONE',  ( 1.000000000000000000, 0.000000000000000000, -3.469446951953616654E-16 ) ) ;
#1730 = CARTESIAN_POINT ( 'NONE',  ( -5.279047395330986450E-15, -24.15089531396988320, -2.156937122105551108 ) ) ;
#1731 =( GEOMETRIC_REPRESENTATION_CONTEXT ( 3 ) GLOBAL_UNCERTAINTY_ASSIGNED_CONTEXT ( ( #5628 ) ) GLOBAL_UNIT_ASSIGNED_CONTEXT ( ( #5420, #4026, #8547 ) ) REPRESENTATION_CONTEXT ( 'NONE', 'WORKASPACE' ) );
#1732 = CARTESIAN_POINT ( 'NONE',  ( 0.7188294034286049072, 21.24680007765648426, -2.395093729190366005 ) ) ;
#1733 = VECTOR ( 'NONE', #3727, 1000.000000000000000 ) ;
#1734 = ORIENTED_EDGE ( 'NONE', *, *, #7963, .F. ) ;
#1735 = CARTESIAN_POINT ( 'NONE',  ( 3.481649420246370141, 19.12180007765648071, -1.193696214020541602 ) ) ;
#1736 = ADVANCED_FACE ( 'NONE', ( #1482 ), #16973, .F. ) ;
#1737 = CYLINDRICAL_SURFACE ( 'NONE', #18184, 2.149999999999995470 ) ;
#1738 = EDGE_CURVE ( 'NONE', #8602, #11760, #86, .T. ) ;
#1739 = CARTESIAN_POINT ( 'NONE',  ( -2.798362969681409851, 17.25319992234354416, -2.102939460078765421 ) ) ;
#1740 =( BOUNDED_CURVE ( )  B_SPLINE_CURVE ( 2, ( #10773, #865, #689, #6334, #6420, #12159, #6604, #9107, #15143 ),
 .UNSPECIFIED., .F., .T. ) 
 B_SPLINE_CURVE_WITH_KNOTS ( ( 3, 2, 2, 2, 3 ),
 ( 0.5775862068965517127, 0.5804597701149425415, 0.5862068965517240882, 0.5919540229885057459, 0.5948275862068965747 ),
 .UNSPECIFIED. ) 
 CURVE ( )  GEOMETRIC_REPRESENTATION_ITEM ( )  RATIONAL_B_SPLINE_CURVE ( ( 0.9330127018922194093, 0.9330127018922194093, 1.000000000000000000, 0.8660254037844387076, 1.000000000000000000, 0.8660254037844387076, 1.000000000000000000, 0.9330127018922194093, 0.9330127018922194093 ) ) 
 REPRESENTATION_ITEM ( '' )  );
#1741 = ORIENTED_EDGE ( 'NONE', *, *, #14309, .T. ) ;
#1742 = B_SPLINE_CURVE_WITH_KNOTS ( 'NONE', 3,
 ( #7246, #5865, #17304, #1438, #216, #12735, #11513, #4476, #11331, #14401, #10119, #1344, #15801, #17024, #2913, #8546, #6976, #14221, #12638, #16933 ),
 .UNSPECIFIED., .F., .F.,
 ( 4, 2, 2, 2, 2, 2, 2, 2, 2, 4 ),
 ( 0.004985757390083797244, 0.005047933101378701548, 0.005110108812673605852, 0.005234460235263413592, 0.005483163080443029073, 0.005980568770802258301, 0.006975380151520719357, 0.007970191532239179547, 0.008467597222598410509, 0.008965002912957639736 ),
 .UNSPECIFIED. ) ;
#1743 = CARTESIAN_POINT ( 'NONE',  ( -4.243569643750004339, -26.14381059887672976, -8.784260816366916913 ) ) ;
#1744 = EDGE_CURVE ( 'NONE', #11984, #10307, #172, .T. ) ;
#1745 = CARTESIAN_POINT ( 'NONE',  ( -4.499999999999999112, 32.99680007765648071, 0.05647727720537927543 ) ) ;
#1746 = ORIENTED_EDGE ( 'NONE', *, *, #2967, .F. ) ;
#1747 = EDGE_CURVE ( 'NONE', #13697, #17672, #3242, .T. ) ;
#1748 = AXIS2_PLACEMENT_3D ( 'NONE', #8901, #11773, #17469 ) ;
#1749 = DIRECTION ( 'NONE',  ( 0.000000000000000000, 0.000000000000000000, 1.000000000000000000 ) ) ;
#1750 = AXIS2_PLACEMENT_3D ( 'NONE', #2805, #6779, #12435 ) ;
#1751 = CARTESIAN_POINT ( 'NONE',  ( -3.999999999999997335, -20.62655511095648109, -9.202611407326488191 ) ) ;
#1752 = CARTESIAN_POINT ( 'NONE',  ( 4.243569643750003451, -23.80763393753414903, -13.99083499735581171 ) ) ;
#1753 = DIRECTION ( 'NONE',  ( 0.000000000000000000, -0.5000000000000011102, -0.8660254037844380415 ) ) ;
#1754 = LINE ( 'NONE', #357, #10644 ) ;
#1755 = CARTESIAN_POINT ( 'NONE',  ( -4.000000000000000888, -25.01336322148850044, -11.44130475926444745 ) ) ;
#1756 = CARTESIAN_POINT ( 'NONE',  ( -4.243569643749997233, -19.59184713035399383, -7.970067471831701056 ) ) ;
#1757 = ORIENTED_EDGE ( 'NONE', *, *, #10319, .T. ) ;
#1758 = CARTESIAN_POINT ( 'NONE',  ( 4.000000000000003553, -19.09940784846689610, -7.021619088400267827 ) ) ;
#1759 = CARTESIAN_POINT ( 'NONE',  ( 4.898587196589413815E-16, 2.700915433685006750, 35.11257424290206330 ) ) ;
#1760 = ORIENTED_EDGE ( 'NONE', *, *, #16945, .T. ) ;
#1761 = VERTEX_POINT ( 'NONE', #17446 ) ;
#1762 = DIRECTION ( 'NONE',  ( -1.000000000000000000, 0.000000000000000000, 4.336808689942021680E-16 ) ) ;
#1763 = CARTESIAN_POINT ( 'NONE',  ( -10.00000000000000000, 20.99999999999999289, 2.499999999999996003 ) ) ;
#1764 =( NAMED_UNIT ( * ) PLANE_ANGLE_UNIT ( ) SI_UNIT ( $, .RADIAN. ) );
#1765 = VECTOR ( 'NONE', #16029, 1000.000000000000000 ) ;
#1766 = CARTESIAN_POINT ( 'NONE',  ( -2.733110507866328476, 29.87819992234354416, -3.862833514489096398 ) ) ;
#1767 = CARTESIAN_POINT ( 'NONE',  ( 3.481649420246395010, 30.87819992234354061, 1.193696214020467439 ) ) ;
#1768 = TOROIDAL_SURFACE ( 'NONE', #14807, 9.000000000000003553, 0.9999999999999991118 ) ;
#1769 = CARTESIAN_POINT ( 'NONE',  ( 2.055738996568313048, 39.49680007765648071, 1.423772053676023441 ) ) ;
#1770 = ORIENTED_EDGE ( 'NONE', *, *, #6248, .F. ) ;
#1771 = CARTESIAN_POINT ( 'NONE',  ( 0.05938372350919016857, 37.62819992234354771, -4.731580009072201776 ) ) ;
#1772 = CARTESIAN_POINT ( 'NONE',  ( -2.000000000000005773, -24.96876754848942070, -5.338138677143647648 ) ) ;
#1773 = EDGE_LOOP ( 'NONE', ( #15553, #2723 ) ) ;
#1774 = LINE ( 'NONE', #3156, #12675 ) ;
#1775 =( BOUNDED_CURVE ( )  B_SPLINE_CURVE ( 3, ( #11679, #6405, #4737, #8900 ),
 .UNSPECIFIED., .F., .F. ) 
 B_SPLINE_CURVE_WITH_KNOTS ( ( 4, 4 ),
 ( 2.111895852752043279, 4.171289454427544285 ),
 .UNSPECIFIED. ) 
 CURVE ( )  GEOMETRIC_REPRESENTATION_ITEM ( )  RATIONAL_B_SPLINE_CURVE ( ( 1.000000000000000000, 0.6767191690918086255, 0.6767191690918086255, 1.000000000000000000 ) ) 
 REPRESENTATION_ITEM ( '' )  );
#1776 = CARTESIAN_POINT ( 'NONE',  ( -0.05938372350927861171, 26.12180007765647005, -3.680117784833935701 ) ) ;
#1777 = CARTESIAN_POINT ( 'NONE',  ( -9.350946484394057734, -10.00000000000000178, 13.61740000484205915 ) ) ;
#1778 = VECTOR ( 'NONE', #10163, 1000.000000000000000 ) ;
#1779 = CARTESIAN_POINT ( 'NONE',  ( 4.243569643749997233, -23.44441649529964877, -4.929126507931827383 ) ) ;
#1780 = CARTESIAN_POINT ( 'NONE',  ( 2.733110507866247652, 31.37180007765647716, -3.862833514489153686 ) ) ;
#1781 = FACE_BOUND ( 'NONE', #14611, .T. ) ;
#1782 = VERTEX_POINT ( 'NONE', #10171 ) ;
#1783 = CARTESIAN_POINT ( 'NONE',  ( 1.027846397803542144, 31.24680007765647716, -3.346150245485522312 ) ) ;
#1784 = CYLINDRICAL_SURFACE ( 'NONE', #13376, 0.9999999999999991118 ) ;
#1785 = FACE_OUTER_BOUND ( 'NONE', #17905, .T. ) ;
#1786 = DIRECTION ( 'NONE',  ( -1.000000000000000000, 0.000000000000000000, 4.336808689942021680E-16 ) ) ;
#1787 = VERTEX_POINT ( 'NONE', #17543 ) ;
#1788 = CARTESIAN_POINT ( 'NONE',  ( 2.115076519116426024, 16.12819992234354416, 3.012182706137062294 ) ) ;
#1789 = DIRECTION ( 'NONE',  ( -0.000000000000000000, -1.000000000000000000, -0.000000000000000000 ) ) ;
#1790 = CARTESIAN_POINT ( 'NONE',  ( 2.121784821875004390, -18.62063887048139321, -8.718783387183849598 ) ) ;
#1791 = CARTESIAN_POINT ( 'NONE',  ( -1.593127413382998459, 15.87180007765648071, -2.091722143975139669 ) ) ;
#1792 = CARTESIAN_POINT ( 'NONE',  ( 3.481649420246394122, 35.87819992234353350, 1.193696214020467439 ) ) ;
#1793 = CARTESIAN_POINT ( 'NONE',  ( -5.330712181944246111E-15, -30.68883019856478711, -11.00373138662392236 ) ) ;
#1794 = FACE_OUTER_BOUND ( 'NONE', #15943, .T. ) ;
#1795 = EDGE_CURVE ( 'NONE', #2086, #16968, #8361, .T. ) ;
#1796 = CARTESIAN_POINT ( 'NONE',  ( -4.243569643750000786, -23.12593826097332794, -8.745782564029356720 ) ) ;
#1797 = DIRECTION ( 'NONE',  ( -0.000000000000000000, 1.000000000000000000, -0.000000000000000000 ) ) ;
#1798 = DIRECTION ( 'NONE',  ( 1.000000000000000000, 0.000000000000000000, 0.000000000000000000 ) ) ;
#1799 = CIRCLE ( 'NONE', #16312, 0.9999999999999991118 ) ;
#1800 = LINE ( 'NONE', #11327, #7109 ) ;
#1801 = DIRECTION ( 'NONE',  ( -1.000000000000000000, 0.000000000000000000, 0.000000000000000000 ) ) ;
#1802 = ORIENTED_EDGE ( 'NONE', *, *, #4978, .T. ) ;
#1803 = ORIENTED_EDGE ( 'NONE', *, *, #5917, .F. ) ;
#1804 = DIRECTION ( 'NONE',  ( 0.000000000000000000, 0.000000000000000000, 1.000000000000000000 ) ) ;
#1805 = CARTESIAN_POINT ( 'NONE',  ( 4.000000000000000888, -25.65863671238343358, -12.36285080908956502 ) ) ;
#1806 = VERTEX_POINT ( 'NONE', #4812 ) ;
#1807 = CARTESIAN_POINT ( 'NONE',  ( -0.05938372350921170689, 18.87819992234354416, 2.628655560595669183 ) ) ;
#1808 = CARTESIAN_POINT ( 'NONE',  ( -5.330712181944245322E-15, -29.88223833494613402, -9.851798824342527183 ) ) ;
#1809 = DIRECTION ( 'NONE',  ( 0.000000000000000000, 0.000000000000000000, 1.000000000000000000 ) ) ;
#1810 = LINE ( 'NONE', #4763, #17017 ) ;
#1811 = ADVANCED_FACE ( 'NONE', ( #6100 ), #17256, .F. ) ;
#1812 = CARTESIAN_POINT ( 'NONE',  ( 5.679766210340737587, -14.60833734475391665, -5.139172057956870709 ) ) ;
#1813 = EDGE_LOOP ( 'NONE', ( #2295, #17707 ) ) ;
#1814 = AXIS2_PLACEMENT_3D ( 'NONE', #5071, #6646, #10726 ) ;
#1815 = CARTESIAN_POINT ( 'NONE',  ( 2.864755990943265829, 36.99680007765648071, 2.011557305968487697 ) ) ;
#1816 = CARTESIAN_POINT ( 'NONE',  ( 4.243569643750000786, -26.35230571544794387, -13.35351281315494987 ) ) ;
#1817 = CARTESIAN_POINT ( 'NONE',  ( -4.000000000000000888, -24.23903503241459845, -10.33544949947430425 ) ) ;
#1818 = CARTESIAN_POINT ( 'NONE',  ( -4.243569643750004339, -28.17642209519573271, -11.68713087331604150 ) ) ;
#1819 = DIRECTION ( 'NONE',  ( -0.000000000000000000, -1.000000000000000000, -0.000000000000000000 ) ) ;
#1820 = DIRECTION ( 'NONE',  ( -0.000000000000000000, -1.000000000000000000, -0.000000000000000000 ) ) ;
#1821 = CARTESIAN_POINT ( 'NONE',  ( 3.999999999999996447, -27.89453318800893555, -11.52972399695732442 ) ) ;
#1822 = CARTESIAN_POINT ( 'NONE',  ( -4.243569643749997233, -22.91500560846283463, -12.71602962843106432 ) ) ;
#1823 = LINE ( 'NONE', #15822, #7712 ) ;
#1824 = CARTESIAN_POINT ( 'NONE',  ( 2.000000000000004441, -17.16411318991132617, -6.270890832864717268 ) ) ;
#1825 = AXIS2_PLACEMENT_3D ( 'NONE', #16288, #2288, #9039 ) ;
#1826 = CARTESIAN_POINT ( 'NONE',  ( 1.497042530366477164, 21.37180007765648071, -2.161531897785062384 ) ) ;
#1827 = ORIENTED_EDGE ( 'NONE', *, *, #4057, .F. ) ;
#1828 = CARTESIAN_POINT ( 'NONE',  ( -3.518350579753630303, 23.12180007765647716, -1.080741659609802952 ) ) ;
#1829 = LINE ( 'NONE', #11726, #3633 ) ;
#1830 = CARTESIAN_POINT ( 'NONE',  ( 0.000000000000000000, 0.000000000000000000, 0.000000000000000000 ) ) ;
#1831 = CARTESIAN_POINT ( 'NONE',  ( 2.000000000000004441, -23.35873870250257767, -15.11773291118586293 ) ) ;
#1832 = LINE ( 'NONE', #7558, #4246 ) ;
#1833 = CARTESIAN_POINT ( 'NONE',  ( -2.798362969681409851, 22.25319992234354416, -2.102939460078765421 ) ) ;
#1834 = VERTEX_POINT ( 'NONE', #9162 ) ;
#1835 = CARTESIAN_POINT ( 'NONE',  ( 4.243569643750000786, -23.77121175186825752, -9.667328613854474284 ) ) ;
#1836 = CARTESIAN_POINT ( 'NONE',  ( 4.481649420246366589, 39.12180007765647360, -1.518615910253458212 ) ) ;
#1837 = ORIENTED_EDGE ( 'NONE', *, *, #4785, .T. ) ;
#1838 = MECHANICAL_DESIGN_GEOMETRIC_PRESENTATION_REPRESENTATION (  '', ( #15169 ), #7739 ) ;
#1839 = CARTESIAN_POINT ( 'NONE',  ( -3.706921591972381904E-14, -18.18775084441045209, -8.667107230630458403 ) ) ;
#1840 = DIRECTION ( 'NONE',  ( 0.000000000000000000, 0.000000000000000000, 1.000000000000000000 ) ) ;
#1841 = EDGE_CURVE ( 'NONE', #8838, #17169, #10437, .T. ) ;
#1842 = CARTESIAN_POINT ( 'NONE',  ( -2.121784821874996396, -22.99774405038527547, -14.96993742516424497 ) ) ;
#1843 = CARTESIAN_POINT ( 'NONE',  ( 0.000000000000000000, 36.39999999999999147, 2.500000000000000000 ) ) ;
#1844 = CARTESIAN_POINT ( 'NONE',  ( 5.040478647146456659, -10.97734431112249887, 19.36653379754666560 ) ) ;
#1845 = EDGE_CURVE ( 'NONE', #15990, #1204, #16138, .T. ) ;
#1846 = CARTESIAN_POINT ( 'NONE',  ( -9.184850993605147944E-16, 13.00000000000000178, -2.500000000000000000 ) ) ;
#1847 = CARTESIAN_POINT ( 'NONE',  ( -2.121784821875005722, -25.06089824606716476, -5.101956642404802622 ) ) ;
#1848 = ORIENTED_EDGE ( 'NONE', *, *, #15782, .F. ) ;
#1849 = CARTESIAN_POINT ( 'NONE',  ( -1.661723472263481630E-14, -20.31715336506863423, -11.70820919606011579 ) ) ;
#1850 = FACE_OUTER_BOUND ( 'NONE', #1901, .T. ) ;
#1851=STYLED_ITEM('',(#18417),#1642);
#1852 = DIRECTION ( 'NONE',  ( 0.000000000000000000, 0.000000000000000000, -1.000000000000000000 ) ) ;
#1853 = ORIENTED_EDGE ( 'NONE', *, *, #3887, .F. ) ;
#1854 = ORIENTED_EDGE ( 'NONE', *, *, #15457, .T. ) ;
#1855 =( BOUNDED_CURVE ( )  B_SPLINE_CURVE ( 2, ( #3393, #9033, #1725, #7358, #9220 ),
 .UNSPECIFIED., .F., .T. ) 
 B_SPLINE_CURVE_WITH_KNOTS ( ( 3, 2, 3 ),
 ( 0.9913793103448276245, 0.9942528735632183423, 0.9961881965693012431 ),
 .UNSPECIFIED. ) 
 CURVE ( )  GEOMETRIC_REPRESENTATION_ITEM ( )  RATIONAL_B_SPLINE_CURVE ( ( 0.9330127018922194093, 0.9330127018922206306, 1.000000000000000000, 0.9548845634181245545, 0.9401540307727882517 ) ) 
 REPRESENTATION_ITEM ( '' )  );
#1856 = CARTESIAN_POINT ( 'NONE',  ( 4.000000000000000888, -24.17450768403005767, -10.24329489549855410 ) ) ;
#1857 = DIRECTION ( 'NONE',  ( -1.000000000000000000, 0.000000000000000000, 4.336808689942021680E-16 ) ) ;
#1858 = MECHANICAL_DESIGN_GEOMETRIC_PRESENTATION_REPRESENTATION (  '', ( #2153 ), #681 ) ;
#1859 = EDGE_CURVE ( 'NONE', #1058, #3578, #3346, .T. ) ;
#1860 = CARTESIAN_POINT ( 'NONE',  ( 4.518350579753602325, 28.12819992234354416, -1.405661355842793725 ) ) ;
#1861 = CARTESIAN_POINT ( 'NONE',  ( 3.500000000000000444, 28.25319992234354416, 0.05647727720529520379 ) ) ;
#1862 = CARTESIAN_POINT ( 'NONE',  ( -0.05938372350921170689, 21.37819992234354416, 2.628655560595669183 ) ) ;
#1863 = CONICAL_SURFACE ( 'NONE', #11899, 2.000000000000001776, 1.029744260000000189 ) ;
#1864 = ORIENTED_EDGE ( 'NONE', *, *, #10960, .T. ) ;
#1865 = CARTESIAN_POINT ( 'NONE',  ( -0.05938372350928957516, 18.62180007765647716, -4.731580009072201776 ) ) ;
#1866 = CARTESIAN_POINT ( 'NONE',  ( -3.999999999999997335, -20.30391836480407619, -8.741838381407161407 ) ) ;
#1867 = EDGE_LOOP ( 'NONE', ( #7751, #5084, #735, #6442 ) ) ;
#1868 = AXIS2_PLACEMENT_3D ( 'NONE', #10362, #2044, #8979 ) ;
#1869 = CARTESIAN_POINT ( 'NONE',  ( 0.000000000000000000, 27.59999999999999432, 2.500000000000000000 ) ) ;
#1870 = VECTOR ( 'NONE', #12957, 1000.000000000000000 ) ;
#1871 = CARTESIAN_POINT ( 'NONE',  ( 1.135272562821090458, 29.74680007765647716, 3.311245368580554072 ) ) ;
#1872 = CARTESIAN_POINT ( 'NONE',  ( -7.736359789466761505, -10.27164672540018309, 8.681487574489553438 ) ) ;
#1873 = CARTESIAN_POINT ( 'NONE',  ( -4.243569643750004339, -23.27234356439432972, -4.683380894645134518 ) ) ;
#1874 = ADVANCED_FACE ( 'NONE', ( #11946 ), #6876, .T. ) ;
#1875 = CARTESIAN_POINT ( 'NONE',  ( -4.518350579753632523, 33.12180007765647360, -1.405661355842698468 ) ) ;
#1876 = CARTESIAN_POINT ( 'NONE',  ( 4.000000000000000000, 1.759474945355381514, -3.047500000000001652 ) ) ;
#1877 = EDGE_LOOP ( 'NONE', ( #13570, #13814, #12192, #17396 ) ) ;
#1878 = CARTESIAN_POINT ( 'NONE',  ( 0.05938372350927906274, 29.87180007765648071, 3.680117784833935701 ) ) ;
#1879 = CARTESIAN_POINT ( 'NONE',  ( -4.000000000000003553, -2.343145750507614533, 25.02027108472330141 ) ) ;
#1880 = FACE_OUTER_BOUND ( 'NONE', #2980, .T. ) ;
#1881 = AXIS2_PLACEMENT_3D ( 'NONE', #14582, #10196, #18241 ) ;
#1882 = FACE_OUTER_BOUND ( 'NONE', #13197, .T. ) ;
#1883 = CARTESIAN_POINT ( 'NONE',  ( -1.661723472263481630E-14, -21.54317299706404754, -13.45914668972107897 ) ) ;
#1884 = EDGE_LOOP ( 'NONE', ( #14599, #5933, #16408, #14556 ) ) ;
#1885=STYLED_ITEM('',(#18389),#2427);
#1886 = CARTESIAN_POINT ( 'NONE',  ( 2.798362969681409851, 28.50319992234354416, 2.102939460078764977 ) ) ;
#1887 = DIRECTION ( 'NONE',  ( -0.000000000000000000, -1.000000000000000000, -0.000000000000000000 ) ) ;
#1888 = CARTESIAN_POINT ( 'NONE',  ( -4.243569643749997233, -19.81769285216720888, -8.292608589270493269 ) ) ;
#1889 = CARTESIAN_POINT ( 'NONE',  ( -1.989345975306426206, 20.24680007765648071, 1.515154207786343799 ) ) ;
#1890 = CARTESIAN_POINT ( 'NONE',  ( -1.027846397803611866, 32.50319992234354771, -3.346150245485499219 ) ) ;
#1891 = CARTESIAN_POINT ( 'NONE',  ( 4.243569643750003451, -24.58196212660805458, -15.09669025714595314 ) ) ;
#1892 =( BOUNDED_CURVE ( )  B_SPLINE_CURVE ( 2, ( #13286, #17587, #9206, #3560, #1995, #693, #16358, #9113, #598 ),
 .UNSPECIFIED., .F., .F. ) 
 B_SPLINE_CURVE_WITH_KNOTS ( ( 3, 2, 2, 2, 3 ),
 ( 0.8534482758620689502, 0.8563218390804597790, 0.8620689655172413257, 0.8678160919540229834, 0.8706896551724138122 ),
 .UNSPECIFIED. ) 
 CURVE ( )  GEOMETRIC_REPRESENTATION_ITEM ( )  RATIONAL_B_SPLINE_CURVE ( ( 0.9330127018922194093, 0.9330127018922194093, 1.000000000000000000, 0.8660254037844387076, 1.000000000000000000, 0.8660254037844387076, 1.000000000000000000, 0.9330127018922194093, 0.9330127018922194093 ) ) 
 REPRESENTATION_ITEM ( '' )  );
#1893 = CARTESIAN_POINT ( 'NONE',  ( -5.279047395330986450E-15, -30.28099347676669240, -10.91162459443741817 ) ) ;
#1894 = CARTESIAN_POINT ( 'NONE',  ( 4.243569643750003451, -19.93599299216462484, -8.461558698405095669 ) ) ;
#1895 = EDGE_CURVE ( 'NONE', #12298, #3719, #14461, .T. ) ;
#1896 = DIRECTION ( 'NONE',  ( 0.000000000000000000, 0.000000000000000000, -1.000000000000000000 ) ) ;
#1897 = AXIS2_PLACEMENT_3D ( 'NONE', #5629, #11272, #7371 ) ;
#1898 = DIRECTION ( 'NONE',  ( 0.000000000000000000, 0.000000000000000000, -1.000000000000000000 ) ) ;
#1899 = CARTESIAN_POINT ( 'NONE',  ( 1.999999999999994449, -23.11898354125731458, -2.696373334311634284 ) ) ;
#1900 = CARTESIAN_POINT ( 'NONE',  ( 9.000000000000005329, 34.19999999999999574, 2.499999999999997335 ) ) ;
#1901 = EDGE_LOOP ( 'NONE', ( #7877, #7597, #7826, #3052 ) ) ;
#1902 = EDGE_LOOP ( 'NONE', ( #12853, #6335, #1332, #1746, #7433 ) ) ;
#1903 = CARTESIAN_POINT ( 'NONE',  ( 4.243569643750000786, -19.86730713195397868, -4.091975012412500945 ) ) ;
#1904 = DIRECTION ( 'NONE',  ( -0.000000000000000000, -1.000000000000000000, -0.000000000000000000 ) ) ;
#1905 = CARTESIAN_POINT ( 'NONE',  ( -8.500000000000005329, 0.000000000000000000, 20.49999999999999645 ) ) ;
#1906 = ORIENTED_EDGE ( 'NONE', *, *, #62, .F. ) ;
#1907 = CARTESIAN_POINT ( 'NONE',  ( -2.518350579753611207, 29.37819992234355126, 0.7558219633769609480 ) ) ;
#1908 = CARTESIAN_POINT ( 'NONE',  ( 4.730628863548789710E-15, -21.72540816142837983, -15.28859851726467589 ) ) ;
#1909 = CARTESIAN_POINT ( 'NONE',  ( -3.500000000000000444, 17.99680007765647716, 0.05647727720536892260 ) ) ;
#1910 = AXIS2_PLACEMENT_3D ( 'NONE', #10415, #8929, #785 ) ;
#1911 = PRODUCT ( 'coil', 'coil', '', ( #8018 ) ) ;
#1912 = FACE_OUTER_BOUND ( 'NONE', #18168, .T. ) ;
#1913 = CARTESIAN_POINT ( 'NONE',  ( 4.242943609565477558, -15.02914320863476405, -7.979206348031381957 ) ) ;
#1914 = ORIENTED_EDGE ( 'NONE', *, *, #14897, .T. ) ;
#1915 = CARTESIAN_POINT ( 'NONE',  ( 2.798362969681366330, 36.49680007765648071, -2.102939460078824929 ) ) ;
#1916 = CARTESIAN_POINT ( 'NONE',  ( -4.243569643749997233, -24.75403505751336297, -15.34243587043265755 ) ) ;
#1917 = EDGE_CURVE ( 'NONE', #2431, #13322, #9840, .T. ) ;
#1918 = DIRECTION ( 'NONE',  ( 0.000000000000000000, 0.000000000000000000, 1.000000000000000000 ) ) ;
#1919 = CARTESIAN_POINT ( 'NONE',  ( 4.730628863548789710E-15, -19.91864238692259903, -12.70826957775434174 ) ) ;
#1920 = DIRECTION ( 'NONE',  ( -0.000000000000000000, 1.000000000000000000, -0.000000000000000000 ) ) ;
#1921 = EDGE_CURVE ( 'NONE', #17611, #11426, #378, .T. ) ;
#1922 = DIRECTION ( 'NONE',  ( 0.000000000000000000, 0.000000000000000000, 1.000000000000000000 ) ) ;
#1923 = EDGE_CURVE ( 'NONE', #4547, #7574, #10132, .T. ) ;
#1924 = DIRECTION ( 'NONE',  ( 0.000000000000000000, 0.000000000000000000, 1.000000000000000000 ) ) ;
#1925 = CARTESIAN_POINT ( 'NONE',  ( 2.121784821874994176, -26.27616332058593684, -6.837535036242106123 ) ) ;
#1926 = DIRECTION ( 'NONE',  ( 0.000000000000000000, 0.000000000000000000, -1.000000000000000000 ) ) ;
#1927 = CARTESIAN_POINT ( 'NONE',  ( 4.299564228933482956E-15, -17.21984060877302269, -7.284788156899542066 ) ) ;
#1928 = ADVANCED_FACE ( 'NONE', ( #366 ), #649, .F. ) ;
#1929 = CARTESIAN_POINT ( 'NONE',  ( 2.481649420246374138, 34.12180007765647360, -0.8687765177876252132 ) ) ;
#1930 = CARTESIAN_POINT ( 'NONE',  ( 0.000000000000000000, 9.254131787996968228, 30.52396275209373044 ) ) ;
#1931 = CARTESIAN_POINT ( 'NONE',  ( 0.05938372350927906967, 24.87180007765647360, 3.680117784833935701 ) ) ;
#1932 = LINE ( 'NONE', #4780, #10114 ) ;
#1933 = CARTESIAN_POINT ( 'NONE',  ( 0.000000000000000000, 0.000000000000000000, 0.000000000000000000 ) ) ;
#1934 = CARTESIAN_POINT ( 'NONE',  ( 4.713407268011036227E-15, -22.90757307230037654, -16.48656056924132329 ) ) ;
#1935 = CARTESIAN_POINT ( 'NONE',  ( 0.000000000000000000, 5.000000000000000000, 2.499999999999999556 ) ) ;
#1936 = CARTESIAN_POINT ( 'NONE',  ( 3.518350579753605434, 15.62819992234354416, -1.080741659609877114 ) ) ;
#1937 = ORIENTED_EDGE ( 'NONE', *, *, #18156, .T. ) ;
#1938 = CARTESIAN_POINT ( 'NONE',  ( 4.243569643749997233, -25.28344594435018777, -7.555532749933419723 ) ) ;
#1939 = CARTESIAN_POINT ( 'NONE',  ( -3.481649420246369697, 20.37180007765647716, 1.193696214020542490 ) ) ;
#1940 = EDGE_LOOP ( 'NONE', ( #7830, #2785, #12942 ) ) ;
#1941 = CYLINDRICAL_SURFACE ( 'NONE', #9557, 0.9999999999999991118 ) ;
#1942 = FACE_OUTER_BOUND ( 'NONE', #17721, .T. ) ;
#1943 = CARTESIAN_POINT ( 'NONE',  ( -4.243569643749997233, -22.94726928300758217, -12.76210693092232162 ) ) ;
#1944 = CARTESIAN_POINT ( 'NONE',  ( 4.000000000000000888, -26.69107429781530527, -13.83732448880975419 ) ) ;
#1945 = CARTESIAN_POINT ( 'NONE',  ( -1.734723475976807094E-15, 43.00000000000000000, -2.500000000000000000 ) ) ;
#1946 = CARTESIAN_POINT ( 'NONE',  ( -6.158835246850665095E-15, -22.12391913957442569, -14.28853813557044639 ) ) ;
#1947 = CARTESIAN_POINT ( 'NONE',  ( -4.243569643749997233, -18.30130014856414533, -6.126975372181463264 ) ) ;
#1948 = ORIENTED_EDGE ( 'NONE', *, *, #13369, .T. ) ;
#1949 = CARTESIAN_POINT ( 'NONE',  ( -4.000000000000007105, 6.938893903907228378E-15, 30.00000000000000000 ) ) ;
#1950 = CARTESIAN_POINT ( 'NONE',  ( -3.999999999999997335, -21.14277390367241694, -9.939848247186581887 ) ) ;
#1951 = CARTESIAN_POINT ( 'NONE',  ( -5.577813053751546416E-15, -28.54808079570739920, -9.515617434797091434 ) ) ;
#1952 = ORIENTED_EDGE ( 'NONE', *, *, #1019, .F. ) ;
#1953 = ORIENTED_EDGE ( 'NONE', *, *, #844, .T. ) ;
#1954 = CARTESIAN_POINT ( 'NONE',  ( 0.000000000000000000, 5.977523610840987267, 32.81826849749789687 ) ) ;
#1955 = DIRECTION ( 'NONE',  ( -0.000000000000000000, -0.5735764363510414965, -0.8191520442889950182 ) ) ;
#1956 = CARTESIAN_POINT ( 'NONE',  ( 3.673772985318163098, 23.00319992234354416, -2.599342558261029001 ) ) ;
#1957 = CARTESIAN_POINT ( 'NONE',  ( 2.798362969681409851, 36.00319992234354771, 2.102939460078764977 ) ) ;
#1958 = CARTESIAN_POINT ( 'NONE',  ( 2.518350579753611207, 18.12819992234354416, -0.7558219633769606149 ) ) ;
#1959 = VERTEX_POINT ( 'NONE', #6006 ) ;
#1960 = CARTESIAN_POINT ( 'NONE',  ( -2.733110507866247652, 17.62180007765648071, 3.862833514489154574 ) ) ;
#1961 = CARTESIAN_POINT ( 'NONE',  ( 3.999999999999996447, -23.95836489284496906, -5.908293092017330217 ) ) ;
#1962 = ORIENTED_EDGE ( 'NONE', *, *, #12426, .F. ) ;
#1963 = ADVANCED_FACE ( 'NONE', ( #13238 ), #3428, .T. ) ;
#1964 = CARTESIAN_POINT ( 'NONE',  ( 9.000000000000000000, 31.99999999999999289, -2.500000000000001332 ) ) ;
#1965 = CARTESIAN_POINT ( 'NONE',  ( 2.115076519116362963, 31.37180007765647716, -3.012182706137107147 ) ) ;
#1966 = FACE_OUTER_BOUND ( 'NONE', #11914, .T. ) ;
#1967 = CARTESIAN_POINT ( 'NONE',  ( -4.243569643750004339, -23.01423416803636002, -4.314762474715088558 ) ) ;
#1968 =( BOUNDED_CURVE ( )  B_SPLINE_CURVE ( 2, ( #638, #447, #17626, #6088, #14544, #11738, #10351, #11931, #3321 ),
 .UNSPECIFIED., .F., .T. ) 
 B_SPLINE_CURVE_WITH_KNOTS ( ( 3, 2, 2, 2, 3 ),
 ( 0.2155172413793103592, 0.2183908045977011603, 0.2241379310344827624, 0.2298850574712643646, 0.2327586206896551657 ),
 .UNSPECIFIED. ) 
 CURVE ( )  GEOMETRIC_REPRESENTATION_ITEM ( )  RATIONAL_B_SPLINE_CURVE ( ( 0.9330127018922192983, 0.9330127018922196314, 1.000000000000000000, 0.8660254037844387076, 1.000000000000000000, 0.8660254037844387076, 1.000000000000000000, 0.9330127018922194093, 0.9330127018922194093 ) ) 
 REPRESENTATION_ITEM ( '' )  );
#1969 = CARTESIAN_POINT ( 'NONE',  ( 1.336863392178479160, 33.74680007765647360, -4.297206761780677731 ) ) ;
#1970 = FACE_OUTER_BOUND ( 'NONE', #15511, .T. ) ;
#1971 = ORIENTED_EDGE ( 'NONE', *, *, #14248, .T. ) ;
#1972 = TOROIDAL_SURFACE ( 'NONE', #11129, 9.000000000000001776, 0.9999999999999991118 ) ;
#1973 = CARTESIAN_POINT ( 'NONE',  ( -0.05938372350927861171, 33.62180007765648071, -3.680117784833935701 ) ) ;
#1974 = DIRECTION ( 'NONE',  ( -4.915049848600951133E-16, 0.000000000000000000, -1.000000000000000000 ) ) ;
#1975 = DIRECTION ( 'NONE',  ( 0.000000000000000000, 0.000000000000000000, 1.000000000000000000 ) ) ;
#1976 = ORIENTED_EDGE ( 'NONE', *, *, #5479, .T. ) ;
#1977 = CARTESIAN_POINT ( 'NONE',  ( 1.135272562821020070, 25.25319992234354416, -3.311245368580577164 ) ) ;
#1978 = CARTESIAN_POINT ( 'NONE',  ( 4.898587196589413815E-16, 13.00000000000000178, 4.000000000000000888 ) ) ;
#1979 = CARTESIAN_POINT ( 'NONE',  ( 4.243569643749996345, -23.96063528801558462, -5.666363347791923744 ) ) ;
#1980 = CARTESIAN_POINT ( 'NONE',  ( 1.989345975306426206, 21.49680007765648071, -1.515154207786343799 ) ) ;
#1981 = EDGE_CURVE ( 'NONE', #9801, #3352, #13338, .T. ) ;
#1982 = CARTESIAN_POINT ( 'NONE',  ( -4.518350579753602325, 19.37819992234354061, 1.405661355842794391 ) ) ;
#1983 = CARTESIAN_POINT ( 'NONE',  ( -4.243569643750004339, -28.46679516609844995, -12.10182659573734476 ) ) ;
#1984 = EDGE_CURVE ( 'NONE', #2199, #904, #13092, .T. ) ;
#1985 = CARTESIAN_POINT ( 'NONE',  ( 4.713407268011036227E-15, -21.81060813707406609, -14.91993228353185508 ) ) ;
#1986 = EDGE_CURVE ( 'NONE', #4985, #13359, #1661, .T. ) ;
#1987 = CARTESIAN_POINT ( 'NONE',  ( -4.243569643750005227, -23.30460723893907371, -4.729458197136391817 ) ) ;
#1988 = AXIS2_PLACEMENT_3D ( 'NONE', #15629, #5433, #11080 ) ;
#1989 = FACE_OUTER_BOUND ( 'NONE', #3979, .T. ) ;
#1990 = CARTESIAN_POINT ( 'NONE',  ( -4.000000000000004441, -27.39982351095120805, -10.82320535775130743 ) ) ;
#1991 = LINE ( 'NONE', #9199, #10964 ) ;
#1992 = DIRECTION ( 'NONE',  ( 0.000000000000000000, 0.8191520442889952403, -0.5735764363510413855 ) ) ;
#1993 = ORIENTED_EDGE ( 'NONE', *, *, #1921, .F. ) ;
#1994 = EDGE_LOOP ( 'NONE', ( #11832, #10181, #7563, #17488 ) ) ;
#1995 = CARTESIAN_POINT ( 'NONE',  ( 4.000000000000000888, -20.75455818158202703, -5.359100830418656258 ) ) ;
#1996 = ORIENTED_EDGE ( 'NONE', *, *, #3630, .F. ) ;
#1997 = CARTESIAN_POINT ( 'NONE',  ( -1.989345975306457071, 24.75319992234354416, -1.515154207786300944 ) ) ;
#1998 = FILL_AREA_STYLE_COLOUR ( '', #8028 ) ;
#1999 = VECTOR ( 'NONE', #2736, 1000.000000000000000 ) ;
#2000 = CARTESIAN_POINT ( 'NONE',  ( 4.243569643749996345, -28.09038562974308562, -11.56425806667268752 ) ) ;
#2001 = CARTESIAN_POINT ( 'NONE',  ( 3.518350579753631191, 24.37180007765648071, 1.080741659609802285 ) ) ;
#2002 = DIRECTION ( 'NONE',  ( 0.000000000000000000, -0.8660254037844390407, -0.4999999999999993339 ) ) ;
#2003 = CARTESIAN_POINT ( 'NONE',  ( 1.848264997552677702, -9.999999999999433342, -4.668605916318575133 ) ) ;
#2004 = MANIFOLD_SOLID_BREP ( 'LPattern6[4]', #1693 ) ;
#2005 = CARTESIAN_POINT ( 'NONE',  ( 4.243569643750000786, -25.31986813001606862, -11.87903913343475892 ) ) ;
#2006 = EDGE_CURVE ( 'NONE', #935, #11183, #6094, .T. ) ;
#2007 = CARTESIAN_POINT ( 'NONE',  ( -1.071796769724481457, -21.85428304249762022, -13.90345788098448665 ) ) ;
#2008 = VECTOR ( 'NONE', #15096, 1000.000000000000000 ) ;
#2009 = CARTESIAN_POINT ( 'NONE',  ( -2.121784821875005722, -27.60972853510210001, -8.742063539214022683 ) ) ;
#2010 = CARTESIAN_POINT ( 'NONE',  ( -6.938893903907228378E-15, 6.938893903907228378E-15, 30.00000000000000000 ) ) ;
#2011 = CARTESIAN_POINT ( 'NONE',  ( 0.000000000000000000, 9.254131787996968228, 30.52396275209373044 ) ) ;
#2012 = CARTESIAN_POINT ( 'NONE',  ( 1.300000000000000044, 1.443375672974065216, 7.222237291452134449E-31 ) ) ;
#2013 = CARTESIAN_POINT ( 'NONE',  ( 2.121784821874994176, -27.05049150965984595, -7.943390296032248443 ) ) ;
#2014 = LINE ( 'NONE', #17787, #5367 ) ;
#2015 = CARTESIAN_POINT ( 'NONE',  ( -4.000000000000000888, -19.65759324776559680, -3.792472546722722715 ) ) ;
#2016 = CARTESIAN_POINT ( 'NONE',  ( -2.518350579753628526, 30.62180007765647716, -0.7558219633769075463 ) ) ;
#2017 = ORIENTED_EDGE ( 'NONE', *, *, #17101, .T. ) ;
#2018 = CARTESIAN_POINT ( 'NONE',  ( -2.864755990943265829, 30.74680007765647716, -2.011557305968488141 ) ) ;
#2019 = CARTESIAN_POINT ( 'NONE',  ( 1.071796769724494780, -27.76222590591464723, -8.393300340351034450 ) ) ;
#2020 = APPLICATION_PROTOCOL_DEFINITION ( 'draft international standard', 'automotive_design', 1998, #13285 ) ;
#2021=STYLED_ITEM('',(#18396),#13775);
#2022 = DIRECTION ( 'NONE',  ( 0.000000000000000000, 0.000000000000000000, -1.000000000000000000 ) ) ;
#2023 = VECTOR ( 'NONE', #15820, 1000.000000000000000 ) ;
#2024 = CARTESIAN_POINT ( 'NONE',  ( 1.135272562821020070, 20.25319992234354416, -3.311245368580577164 ) ) ;
#2025 = EDGE_CURVE ( 'NONE', #15490, #11760, #15195, .T. ) ;
#2026 = ORIENTED_EDGE ( 'NONE', *, *, #14309, .F. ) ;
#2027 = CARTESIAN_POINT ( 'NONE',  ( -4.243569643750004339, -24.59515422072892221, -6.572550296786629609 ) ) ;
#2028 = CARTESIAN_POINT ( 'NONE',  ( 0.05938372350929014415, 39.87180007765647360, 4.731580009072201776 ) ) ;
#2029 = ORIENTED_EDGE ( 'NONE', *, *, #6657, .F. ) ;
#2030 = ADVANCED_FACE ( 'NONE', ( #15844 ), #16037, .F. ) ;
#2031 = FACE_OUTER_BOUND ( 'NONE', #14752, .T. ) ;
#2032 = DIRECTION ( 'NONE',  ( 0.000000000000000000, 0.000000000000000000, -1.000000000000000000 ) ) ;
#2033 = CARTESIAN_POINT ( 'NONE',  ( 4.730628863548789710E-15, -20.98334364689921827, -14.22882055996578643 ) ) ;
#2034 = DIRECTION ( 'NONE',  ( 0.000000000000000000, 0.000000000000000000, -1.000000000000000000 ) ) ;
#2035 = VECTOR ( 'NONE', #2363, 1000.000000000000000 ) ;
#2036 = DIRECTION ( 'NONE',  ( 3.469446951953612217E-16, -0.000000000000000000, 1.000000000000000000 ) ) ;
#2037 = CARTESIAN_POINT ( 'NONE',  ( 4.243569643750003451, -24.80780784842128028, -15.41923137458474535 ) ) ;
#2038 = ORIENTED_EDGE ( 'NONE', *, *, #9326, .F. ) ;
#2039 = CARTESIAN_POINT ( 'NONE',  ( -4.000000000000000888, -19.91570264412356650, -4.161090966652770895 ) ) ;
#2040 = CARTESIAN_POINT ( 'NONE',  ( 4.000000000000003553, -20.97070097276710854, -9.694102633899879251 ) ) ;
#2041 = DIRECTION ( 'NONE',  ( 0.000000000000000000, 0.000000000000000000, 1.000000000000000000 ) ) ;
#2042 = ORIENTED_EDGE ( 'NONE', *, *, #609, .T. ) ;
#2043 = EDGE_LOOP ( 'NONE', ( #15478, #17092, #6732, #11472 ) ) ;
#2044 = DIRECTION ( 'NONE',  ( -0.000000000000000000, -0.5735764363510414965, -0.8191520442889950182 ) ) ;
#2045 = DIRECTION ( 'NONE',  ( 0.000000000000000000, -1.000000000000000000, 0.000000000000000000 ) ) ;
#2046 = CARTESIAN_POINT ( 'NONE',  ( 3.673772985318163098, 28.00319992234354771, -2.599342558261029001 ) ) ;
#2047 = CARTESIAN_POINT ( 'NONE',  ( 3.579096709490575479E-14, -23.83758431146952361, -2.788331270066955359 ) ) ;
#2048 = CARTESIAN_POINT ( 'NONE',  ( -2.055738996568281518, 21.75319992234354416, 1.423772053676066962 ) ) ;
#2049 = ORIENTED_EDGE ( 'NONE', *, *, #11410, .F. ) ;
#2050 =( GEOMETRIC_REPRESENTATION_CONTEXT ( 3 ) GLOBAL_UNCERTAINTY_ASSIGNED_CONTEXT ( ( #18116 ) ) GLOBAL_UNIT_ASSIGNED_CONTEXT ( ( #6927, #18002, #16878 ) ) REPRESENTATION_CONTEXT ( 'NONE', 'WORKASPACE' ) );
#2051 = CARTESIAN_POINT ( 'NONE',  ( 4.518350579753602325, 38.12819992234354061, -1.405661355842793725 ) ) ;
#2052 = ADVANCED_FACE ( 'NONE', ( #14456 ), #17582, .T. ) ;
#2053 = VECTOR ( 'NONE', #4732, 1000.000000000000000 ) ;
#2054 = CARTESIAN_POINT ( 'NONE',  ( -4.000000000000004441, -23.52818256558167320, -5.293929058800590504 ) ) ;
#2055 = EDGE_LOOP ( 'NONE', ( #8033, #8313, #8249, #18260 ) ) ;
#2056 = DIRECTION ( 'NONE',  ( 0.000000000000000000, 0.000000000000000000, -1.000000000000000000 ) ) ;
#2057 = CARTESIAN_POINT ( 'NONE',  ( -3.500000000000000444, 37.99680007765647360, 0.05647727720536892260 ) ) ;
#2058 = DIRECTION ( 'NONE',  ( 1.000000000000000000, 0.000000000000000000, -0.000000000000000000 ) ) ;
#2059 = CARTESIAN_POINT ( 'NONE',  ( 2.121784821875004390, -19.13685766319732906, -9.456020227043945070 ) ) ;
#2060 = CARTESIAN_POINT ( 'NONE',  ( -5.330712181944245322E-15, -27.59151744226915781, -6.580310347463352194 ) ) ;
#2061 = PRODUCT_DEFINITION_SHAPE ( 'NONE', 'NONE',  #6725 ) ;
#2062 = CIRCLE ( 'NONE', #2370, 0.9999999999999991118 ) ;
#2063 = CARTESIAN_POINT ( 'NONE',  ( 0.000000000000000000, 15.00000000000000178, 0.000000000000000000 ) ) ;
#2064 = ORIENTED_EDGE ( 'NONE', *, *, #16585, .F. ) ;
#2065 = CARTESIAN_POINT ( 'NONE',  ( 7.971931588564637572, -10.00000000000000178, 17.73270869615947021 ) ) ;
#2066 = DIRECTION ( 'NONE',  ( 0.000000000000000000, 0.000000000000000000, -1.000000000000000000 ) ) ;
#2067 = CARTESIAN_POINT ( 'NONE',  ( 4.000000000000003553, -20.19637278369320299, -8.588247374109734267 ) ) ;
#2068 = CARTESIAN_POINT ( 'NONE',  ( -1.071796769724505882, -19.53129847527590712, -10.58589210161404814 ) ) ;
#2069 = VERTEX_POINT ( 'NONE', #18301 ) ;
#2070 = CARTESIAN_POINT ( 'NONE',  ( 3.481649420246394122, 25.87819992234354771, 1.193696214020467439 ) ) ;
#2071 = CARTESIAN_POINT ( 'NONE',  ( -10.00000000000000000, 29.79999999999999716, 2.499999999999996003 ) ) ;
#2072 = CARTESIAN_POINT ( 'NONE',  ( -4.243569643749997233, -19.04336466309330689, -7.186753329480350061 ) ) ;
#2073 = CARTESIAN_POINT ( 'NONE',  ( 1.989345975306426206, 23.99680007765648071, -1.515154207786343799 ) ) ;
#2074 = CARTESIAN_POINT ( 'NONE',  ( -0.05938372350918959958, 21.37819992234354416, 4.731580009072201776 ) ) ;
#2075 = CARTESIAN_POINT ( 'NONE',  ( 4.243569643750003451, -24.84007152296602428, -15.46530867707600088 ) ) ;
#2076 = CARTESIAN_POINT ( 'NONE',  ( -4.000000000000000888, -26.56201959963631509, -13.65301527884473387 ) ) ;
#2077 = VECTOR ( 'NONE', #8869, 1000.000000000000000 ) ;
#2078 = CARTESIAN_POINT ( 'NONE',  ( -2.121784821875005722, -24.80278884970919506, -4.733338222474753998 ) ) ;
#2079 = CARTESIAN_POINT ( 'NONE',  ( -1.336863392178478716, 37.49680007765647360, 4.297206761780677731 ) ) ;
#2080 = PLANE ( 'NONE',  #12045 ) ;
#2081 = EDGE_CURVE ( 'NONE', #5846, #12141, #3843, .T. ) ;
#2082 = DIRECTION ( 'NONE',  ( 1.000000000000000000, 0.000000000000000000, 0.000000000000000000 ) ) ;
#2083 = EDGE_CURVE ( 'NONE', #3510, #1667, #1151, .T. ) ;
#2084 = DIRECTION ( 'NONE',  ( 1.000000000000000000, 0.000000000000000000, 0.000000000000000000 ) ) ;
#2085 = ORIENTED_EDGE ( 'NONE', *, *, #15852, .F. ) ;
#2086 = VERTEX_POINT ( 'NONE', #17251 ) ;
#2087 = DIRECTION ( 'NONE',  ( -1.000000000000000000, 0.000000000000000000, 0.000000000000000000 ) ) ;
#2088 = CARTESIAN_POINT ( 'NONE',  ( -5.577813053751546416E-15, -28.99977223862889275, -10.16069966866791141 ) ) ;
#2089 = PRESENTATION_STYLE_ASSIGNMENT (( #4571 ) ) ;
#2090 = EDGE_CURVE ( 'NONE', #2141, #13230, #16907, .T. ) ;
#2091 = ORIENTED_EDGE ( 'NONE', *, *, #7137, .F. ) ;
#2092 = CARTESIAN_POINT ( 'NONE',  ( -2.500000000000001332, 29.50319992234354771, -0.05647727720530596601 ) ) ;
#2093 = CARTESIAN_POINT ( 'NONE',  ( 2.121784821874994176, -28.85725728416562674, -10.52371923554258260 ) ) ;
#2094 = CARTESIAN_POINT ( 'NONE',  ( -1.135272562821090014, 20.99680007765647716, -3.311245368580554072 ) ) ;
#2095 = ADVANCED_FACE ( 'NONE', ( #1850 ), #2804, .F. ) ;
#2096 = CARTESIAN_POINT ( 'NONE',  ( -1.734723475976807094E-15, 16.59999999999999787, -12.50000000000000000 ) ) ;
#2097 = CARTESIAN_POINT ( 'NONE',  ( 0.6850780354679415485, -10.00000000000053113, -5.037014450714041303 ) ) ;
#2098 = CARTESIAN_POINT ( 'NONE',  ( 2.121784821875004390, -22.78265288675364175, -14.66275540855586890 ) ) ;
#2099 = EDGE_CURVE ( 'NONE', #13, #16617, #1564, .T. ) ;
#2100 = CIRCLE ( 'NONE', #20, 1.250000000000000222 ) ;
#2101 = LINE ( 'NONE', #14709, #140 ) ;
#2102 = CARTESIAN_POINT ( 'NONE',  ( 4.730628863548789710E-15, -20.17675178328056873, -13.07688799768438948 ) ) ;
#2103 = FACE_BOUND ( 'NONE', #1813, .T. ) ;
#2104 = PRODUCT_DEFINITION ( 'UNKNOWN', '', #1556, #14150 ) ;
#2105 = DIRECTION ( 'NONE',  ( -0.000000000000000000, -0.5735764363510414965, -0.8191520442889950182 ) ) ;
#2106 = DIRECTION ( 'NONE',  ( 0.000000000000000000, 0.000000000000000000, 1.000000000000000000 ) ) ;
#2107 = CARTESIAN_POINT ( 'NONE',  ( -5.330712181944245322E-15, -27.55925376772441382, -6.534233044972094895 ) ) ;
#2108 = ORIENTED_EDGE ( 'NONE', *, *, #10220, .T. ) ;
#2109 = CARTESIAN_POINT ( 'NONE',  ( -12.99999999999999822, 48.00000000000000000, 16.00000000000000000 ) ) ;
#2110 = DIRECTION ( 'NONE',  ( -0.000000000000000000, -0.5735764363510414965, -0.8191520442889950182 ) ) ;
#2111 = CARTESIAN_POINT ( 'NONE',  ( -0.05938372350926768989, 28.62180007765647716, -2.628655560595669183 ) ) ;
#2112 = ORIENTED_EDGE ( 'NONE', *, *, #2025, .F. ) ;
#2113 = CARTESIAN_POINT ( 'NONE',  ( 3.518350579753631191, 29.37180007765647360, 1.080741659609802729 ) ) ;
#2114 = CARTESIAN_POINT ( 'NONE',  ( -1.999999999999996225, -23.83193926249218109, -15.79353334772428497 ) ) ;
#2115 = APPLICATION_PROTOCOL_DEFINITION ( 'draft international standard', 'automotive_design', 1998, #3466 ) ;
#2116 = VECTOR ( 'NONE', #10912, 1000.000000000000000 ) ;
#2117 = DIRECTION ( 'NONE',  ( 0.000000000000000000, 0.000000000000000000, -1.000000000000000000 ) ) ;
#2118 = CARTESIAN_POINT ( 'NONE',  ( -0.05938372350920063936, 21.37819992234353705, 3.680117784833935701 ) ) ;
#2119 = ORIENTED_EDGE ( 'NONE', *, *, #13222, .T. ) ;
#2120 = CARTESIAN_POINT ( 'NONE',  ( -2.121784821874996396, -19.38421250137371388, -9.809279546143578443 ) ) ;
#2121 = CARTESIAN_POINT ( 'NONE',  ( 0.05938372350927906274, 19.87180007765648426, 3.680117784833935701 ) ) ;
#2122 = ORIENTED_EDGE ( 'NONE', *, *, #12585, .F. ) ;
#2123 = FILL_AREA_STYLE ('',( #14731 ) ) ;
#2124 = FACE_OUTER_BOUND ( 'NONE', #10407, .T. ) ;
#2125 = CARTESIAN_POINT ( 'NONE',  ( -3.924030842084162085, -26.26574055918599626, -14.95313944102314707 ) ) ;
#2126 = DIRECTION ( 'NONE',  ( 0.000000000000000000, 0.000000000000000000, 1.000000000000000000 ) ) ;
#2127 = AXIS2_PLACEMENT_3D ( 'NONE', #494, #6042, #12996 ) ;
#2128 = CARTESIAN_POINT ( 'NONE',  ( 7.338942192890510086, -12.39130301598704520, 9.345622607077766375 ) ) ;
#2129 = LINE ( 'NONE', #1091, #2008 ) ;
#2130 = CARTESIAN_POINT ( 'NONE',  ( -4.243569643750005227, -22.01406025714923231, -2.886366097486154469 ) ) ;
#2131 = VERTEX_POINT ( 'NONE', #13143 ) ;
#2132 = LINE ( 'NONE', #6379, #10387 ) ;
#2133 = CARTESIAN_POINT ( 'NONE',  ( 1.999999999999994449, -25.50649545827347353, -6.106093719671341624 ) ) ;
#2134 = EDGE_LOOP ( 'NONE', ( #8973, #7928, #13787, #3984 ) ) ;
#2135 = ORIENTED_EDGE ( 'NONE', *, *, #4168, .F. ) ;
#2136 = CARTESIAN_POINT ( 'NONE',  ( -2.000000000000005773, -24.19443935941551160, -4.232283417353504440 ) ) ;
#2137 = PRESENTATION_STYLE_ASSIGNMENT (( #6384 ) ) ;
#2138 = CARTESIAN_POINT ( 'NONE',  ( -4.481649420246396787, 27.12819992234355126, -1.518615910253363399 ) ) ;
#2139 = CARTESIAN_POINT ( 'NONE',  ( -2.864755990943222308, 39.25319992234354771, 2.011557305968548093 ) ) ;
#2140 = CARTESIAN_POINT ( 'NONE',  ( -0.05938372350921170689, 18.87819992234354416, 2.628655560595669183 ) ) ;
#2141 = VERTEX_POINT ( 'NONE', #11744 ) ;
#2142 = MECHANICAL_DESIGN_GEOMETRIC_PRESENTATION_REPRESENTATION (  '', ( #10995 ), #5379 ) ;
#2143 = CARTESIAN_POINT ( 'NONE',  ( -4.518350579753632523, 20.62180007765647716, -1.405661355842698468 ) ) ;
#2144 = CARTESIAN_POINT ( 'NONE',  ( 4.713407268011036227E-15, -17.93896719170453835, -9.390655984581140814 ) ) ;
#2145 = ORIENTED_EDGE ( 'NONE', *, *, #4551, .T. ) ;
#2146 = LINE ( 'NONE', #7777, #15092 ) ;
#2147 = CARTESIAN_POINT ( 'NONE',  ( 2.115076519116362963, 38.87180007765645939, -3.012182706137107147 ) ) ;
#2148 = CARTESIAN_POINT ( 'NONE',  ( 2.200000000000000178, 0.000000000000000000, 3.799999999999999378 ) ) ;
#2149 = CIRCLE ( 'NONE', #11901, 3.799999999999999378 ) ;
#2150 = ADVANCED_FACE ( 'NONE', ( #14013 ), #17441, .T. ) ;
#2151 = CARTESIAN_POINT ( 'NONE',  ( 4.730628863548789710E-15, -15.78889204519509981, -6.810374858873577075 ) ) ;
#2152 = CARTESIAN_POINT ( 'NONE',  ( -4.243569643750005227, -26.66002939159267271, -9.521497656227012385 ) ) ;
#2153 = STYLED_ITEM ( 'NONE', ( #16017 ), #12694 ) ;
#2154 = CARTESIAN_POINT ( 'NONE',  ( 1.071796769724495224, -23.16788342572513315, -15.77947364994655288 ) ) ;
#2155 = EDGE_CURVE ( 'NONE', #15759, #4478, #2720, .T. ) ;
#2156 = ORIENTED_EDGE ( 'NONE', *, *, #10788, .F. ) ;
#2157 = CARTESIAN_POINT ( 'NONE',  ( 0.000000000000000000, -10.00000000000000178, -12.59063537424807677 ) ) ;
#2158 = DIRECTION ( 'NONE',  ( 0.000000000000000000, 0.000000000000000000, -1.000000000000000000 ) ) ;
#2159 = PLANE ( 'NONE',  #10421 ) ;
#2160 = CARTESIAN_POINT ( 'NONE',  ( 4.243569643750003451, -24.58196212660805458, -15.09669025714595314 ) ) ;
#2161 = ORIENTED_EDGE ( 'NONE', *, *, #3935, .T. ) ;
#2162 = CARTESIAN_POINT ( 'NONE',  ( 3.481649420246394122, 30.87819992234353350, 1.193696214020467439 ) ) ;
#2163 = DIRECTION ( 'NONE',  ( 0.000000000000000000, 0.000000000000000000, 1.000000000000000000 ) ) ;
#2164 = CARTESIAN_POINT ( 'NONE',  ( -2.121784821875005722, -24.51241577880647782, -4.318642500053448963 ) ) ;
#2165 = CARTESIAN_POINT ( 'NONE',  ( -2.055738996568313048, 20.74680007765648071, -1.423772053676023441 ) ) ;
#2166 = AXIS2_PLACEMENT_3D ( 'NONE', #17159, #11467, #1762 ) ;
#2167 = CARTESIAN_POINT ( 'NONE',  ( -1.336863392178569088, 20.00319992234354416, -4.297206761780648421 ) ) ;
#2168=STYLED_ITEM('',(#18417),#1586);
#2169 = CARTESIAN_POINT ( 'NONE',  ( 2.121784821875004390, -23.04076228311161145, -15.03137382848591663 ) ) ;
#2170 = CARTESIAN_POINT ( 'NONE',  ( -1.999999999999996225, -23.50930251633977264, -15.33276032180496173 ) ) ;
#2171 = CARTESIAN_POINT ( 'NONE',  ( 2.121784821875004390, -18.91101194138411046, -9.133479109605152857 ) ) ;
#2172 = CARTESIAN_POINT ( 'NONE',  ( 1.135272562821090458, 17.24680007765647716, 3.311245368580554072 ) ) ;
#2173 = EDGE_CURVE ( 'NONE', #14275, #5635, #6318, .T. ) ;
#2174 = CARTESIAN_POINT ( 'NONE',  ( -9.000000000000001776, 43.00000000000000000, 2.499999999999995559 ) ) ;
#2175 = VECTOR ( 'NONE', #4556, 999.9999999999998863 ) ;
#2176 = CARTESIAN_POINT ( 'NONE',  ( -5.040478647146447777, -15.02265568887750646, -7.935421837999481198 ) ) ;
#2177 = AXIS2_PLACEMENT_3D ( 'NONE', #14843, #4525, #1324 ) ;
#2178 = DIRECTION ( 'NONE',  ( 0.000000000000000000, 0.000000000000000000, 1.000000000000000000 ) ) ;
#2179 = ORIENTED_EDGE ( 'NONE', *, *, #3658, .T. ) ;
#2180 = ORIENTED_EDGE ( 'NONE', *, *, #11064, .F. ) ;
#2181 = FACE_OUTER_BOUND ( 'NONE', #16770, .T. ) ;
#2182 = DIRECTION ( 'NONE',  ( 3.469446951953612217E-16, -0.000000000000000000, 1.000000000000000000 ) ) ;
#2183 = CARTESIAN_POINT ( 'NONE',  ( 3.999999999999996447, -27.83000583821450036, -11.43756939096804714 ) ) ;
#2184 = EDGE_LOOP ( 'NONE', ( #18223, #5378, #6453, #10869 ) ) ;
#2185 = CARTESIAN_POINT ( 'NONE',  ( -2.481649420246391902, 32.12819992234354771, -0.8687765177875723666 ) ) ;
#2186 =( NAMED_UNIT ( * ) PLANE_ANGLE_UNIT ( ) SI_UNIT ( $, .RADIAN. ) );
#2187 = CARTESIAN_POINT ( 'NONE',  ( 2.121784821874994176, -28.34103849144968379, -9.786482395682487123 ) ) ;
#2188 = CARTESIAN_POINT ( 'NONE',  ( -3.481649420246369697, 25.37180007765648071, 1.193696214020542490 ) ) ;
#2189 = CARTESIAN_POINT ( 'NONE',  ( -8.500000000000010658, 13.00000000000000000, 22.64999999999998437 ) ) ;
#2190 = DIRECTION ( 'NONE',  ( 0.000000000000000000, 0.000000000000000000, -1.000000000000000000 ) ) ;
#2191 = EDGE_CURVE ( 'NONE', #5572, #4695, #3256, .T. ) ;
#2192 = VECTOR ( 'NONE', #12760, 1000.000000000000000 ) ;
#2193 = CIRCLE ( 'NONE', #1298, 6.000000000000000000 ) ;
#2194 = CARTESIAN_POINT ( 'NONE',  ( -4.243569643750000786, -25.44892282819504459, -12.06334834339978634 ) ) ;
#2195 = FACE_BOUND ( 'NONE', #2494, .T. ) ;
#2196 = DIRECTION ( 'NONE',  ( -0.000000000000000000, -1.000000000000000000, -0.000000000000000000 ) ) ;
#2197 = LINE ( 'NONE', #13662, #11458 ) ;
#2198 = CARTESIAN_POINT ( 'NONE',  ( 4.243569643750000786, -22.70651049189163828, -8.146777631643026041 ) ) ;
#2199 = VERTEX_POINT ( 'NONE', #11491 ) ;
#2200 = DIRECTION ( 'NONE',  ( -0.000000000000000000, -0.5735764363510414965, -0.8191520442889950182 ) ) ;
#2201 = AXIS2_PLACEMENT_3D ( 'NONE', #11615, #4484, #11424 ) ;
#2202 = CARTESIAN_POINT ( 'NONE',  ( -8.000000000000001776, 36.39999999999999147, 2.499999999999995115 ) ) ;
#2203 = CARTESIAN_POINT ( 'NONE',  ( -1.989345975306426206, 27.74680007765648071, 1.515154207786343799 ) ) ;
#2204 = VERTEX_POINT ( 'NONE', #17186 ) ;
#2205 = CARTESIAN_POINT ( 'NONE',  ( 2.211161402132902243, 29.62180007765647716, 2.942372952327172442 ) ) ;
#2206 = CYLINDRICAL_SURFACE ( 'NONE', #8950, 2.149999999999995470 ) ;
#2207 = CARTESIAN_POINT ( 'NONE',  ( 4.930380657631323784E-32, -31.79590458133957398, -21.12777768298181513 ) ) ;
#2208 = DIRECTION ( 'NONE',  ( -0.000000000000000000, 1.000000000000000000, -0.000000000000000000 ) ) ;
#2209 = EDGE_CURVE ( 'NONE', #18202, #5429, #7480, .T. ) ;
#2210 = EDGE_CURVE ( 'NONE', #4161, #15889, #6899, .T. ) ;
#2211 = ORIENTED_EDGE ( 'NONE', *, *, #8240, .F. ) ;
#2212 = CARTESIAN_POINT ( 'NONE',  ( 2.121784821875004390, -19.16912133774208016, -9.502097529535200593 ) ) ;
#2213 = CARTESIAN_POINT ( 'NONE',  ( -3.518350579753630747, 15.62180007765647538, -1.080741659609802729 ) ) ;
#2214 = ADVANCED_FACE ( 'NONE', ( #8708 ), #13710, .T. ) ;
#2215 = VERTEX_POINT ( 'NONE', #2810 ) ;
#2216 = LINE ( 'NONE', #12198, #5203 ) ;
#2217 = PLANE ( 'NONE',  #16276 ) ;
#2218 = MANIFOLD_SOLID_BREP ( 'M4 Clearance Hole1', #2906 ) ;
#2219 = DIRECTION ( 'NONE',  ( 0.000000000000000000, 0.000000000000000000, 1.000000000000000000 ) ) ;
#2220 = CARTESIAN_POINT ( 'NONE',  ( 6.931282879835348076, -10.37761417744432002, 2.815650091973651126 ) ) ;
#2221 = CARTESIAN_POINT ( 'NONE',  ( 4.299564228933482956E-15, -18.51038759056286054, -9.127880256549779858 ) ) ;
#2222 = AXIS2_PLACEMENT_3D ( 'NONE', #2975, #8699, #14283 ) ;
#2223 = CARTESIAN_POINT ( 'NONE',  ( -2.121784821875005722, -23.51224186791935011, -2.890246122824515318 ) ) ;
#2224 = ORIENTED_EDGE ( 'NONE', *, *, #2965, .T. ) ;
#2225 = CARTESIAN_POINT ( 'NONE',  ( -4.000000000000004441, -25.39947568988189985, -7.966412604300202815 ) ) ;
#2226 = ORIENTED_EDGE ( 'NONE', *, *, #10859, .F. ) ;
#2227 = VERTEX_POINT ( 'NONE', #17 ) ;
#2228 = DIRECTION ( 'NONE',  ( -0.000000000000000000, 1.000000000000000000, -0.000000000000000000 ) ) ;
#2229 =( LENGTH_UNIT ( ) NAMED_UNIT ( * ) SI_UNIT ( .MILLI., .METRE. ) );
#2230 = CARTESIAN_POINT ( 'NONE',  ( 2.829195390882724759, 32.87819992234354771, -3.793023760679264278 ) ) ;
#2231 = CARTESIAN_POINT ( 'NONE',  ( -2.115076519116425580, 34.87819992234354771, -3.012182706137063182 ) ) ;
#2232 = CARTESIAN_POINT ( 'NONE',  ( 0.7188294034286553114, 18.75319992234354416, 2.395093729190349130 ) ) ;
#2233 = ORIENTED_EDGE ( 'NONE', *, *, #12940, .T. ) ;
#2234 = CARTESIAN_POINT ( 'NONE',  ( 3.673772985318163098, 38.00319992234354061, -2.599342558261029001 ) ) ;
#2235 = VECTOR ( 'NONE', #10376, 1000.000000000000000 ) ;
#2236 = CARTESIAN_POINT ( 'NONE',  ( 3.999999999999996447, -22.92592730741309737, -4.433819412297139273 ) ) ;
#2237 = EDGE_LOOP ( 'NONE', ( #4935, #6317, #4510, #1327 ) ) ;
#2238 = CARTESIAN_POINT ( 'NONE',  ( 9.000000000000000000, 20.99999999999999289, -2.500000000000001332 ) ) ;
#2239 = CARTESIAN_POINT ( 'NONE',  ( -3.481649420246369697, 35.37180007765648071, 1.193696214020542490 ) ) ;
#2240 =( BOUNDED_CURVE ( )  B_SPLINE_CURVE ( 3, ( #14878, #2176, #16351, #6510 ),
 .UNSPECIFIED., .F., .F. ) 
 B_SPLINE_CURVE_WITH_KNOTS ( ( 4, 4 ),
 ( 5.253488506341836839, 6.283185307179586232 ),
 .UNSPECIFIED. ) 
 CURVE ( )  GEOMETRIC_REPRESENTATION_ITEM ( )  RATIONAL_B_SPLINE_CURVE ( ( 1.000000000000000000, 0.9135782535825738293, 0.9135782535825738293, 1.000000000000000000 ) ) 
 REPRESENTATION_ITEM ( '' )  );
#2241 = CARTESIAN_POINT ( 'NONE',  ( -8.500000000000005329, 10.00000000000000000, 20.49999999999999645 ) ) ;
#2242 = EDGE_CURVE ( 'NONE', #6649, #8268, #1419, .T. ) ;
#2243 = PLANE ( 'NONE',  #7359 ) ;
#2244 = CARTESIAN_POINT ( 'NONE',  ( 2.121784821875004390, -21.49210590496380036, -12.81966330890563022 ) ) ;
#2245 = CARTESIAN_POINT ( 'NONE',  ( 2.884887816493423518, -29.26500710983614084, -12.65241590468473909 ) ) ;
#2246 = ORIENTED_EDGE ( 'NONE', *, *, #11807, .F. ) ;
#2247 = MANIFOLD_SOLID_BREP ( 'LPattern6[12]', #16538 ) ;
#2248 = CARTESIAN_POINT ( 'NONE',  ( 6.503403972914452602, -9.999999999998879119, 16.98026834952917952 ) ) ;
#2249 = CARTESIAN_POINT ( 'NONE',  ( 4.299564228933482956E-15, -17.15531325897858039, -7.192633550910265683 ) ) ;
#2250 = CARTESIAN_POINT ( 'NONE',  ( 8.499999999999992895, 14.80000000000000071, 20.49999999999999645 ) ) ;
#2251 = CARTESIAN_POINT ( 'NONE',  ( -1.999999999999996225, -19.96029831712264979, -10.26425704877356715 ) ) ;
#2252 = ORIENTED_EDGE ( 'NONE', *, *, #8067, .T. ) ;
#2253 = CARTESIAN_POINT ( 'NONE',  ( -3.500000000000000444, 32.00319992234354771, -0.05647727720529563400 ) ) ;
#2254 = LINE ( 'NONE', #9092, #991 ) ;
#2255 = CARTESIAN_POINT ( 'NONE',  ( -4.243569643750000786, -20.77069001920686375, -5.382139482167671574 ) ) ;
#2256 = CARTESIAN_POINT ( 'NONE',  ( -2.518350579753628526, 20.62180007765647716, -0.7558219633769075463 ) ) ;
#2257 = CARTESIAN_POINT ( 'NONE',  ( -1.336863392178569088, 17.50319992234354771, -4.297206761780648421 ) ) ;
#2258 = CARTESIAN_POINT ( 'NONE',  ( 4.000000000000000888, -26.17485550509936942, -13.10008764894965871 ) ) ;
#2259 = VERTEX_POINT ( 'NONE', #3355 ) ;
#2260 = ADVANCED_FACE ( 'NONE', ( #6121 ), #2893, .F. ) ;
#2261 = CARTESIAN_POINT ( 'NONE',  ( 4.243569643749996345, -22.70235198077049787, -3.869348550632942363 ) ) ;
#2262 = ADVANCED_FACE ( 'NONE', ( #10664 ), #18186, .T. ) ;
#2263 = CARTESIAN_POINT ( 'NONE',  ( -3.673772985318219053, 38.24680007765647360, -2.599342558260952174 ) ) ;
#2264 = AXIS2_PLACEMENT_3D ( 'NONE', #115, #15695, #2993 ) ;
#2265 = DIRECTION ( 'NONE',  ( -0.000000000000000000, -1.000000000000000000, -0.000000000000000000 ) ) ;
#2266 = DIRECTION ( 'NONE',  ( 0.000000000000000000, -1.000000000000000000, 0.000000000000000000 ) ) ;
#2267 = CARTESIAN_POINT ( 'NONE',  ( -10.00000000000000000, 29.79999999999999716, 2.499999999999998224 ) ) ;
#2268 = EDGE_LOOP ( 'NONE', ( #13436, #12204, #9696, #9451 ) ) ;
#2269 = VERTEX_POINT ( 'NONE', #3262 ) ;
#2270 = DIRECTION ( 'NONE',  ( 0.000000000000000000, 0.8191520442889952403, -0.5735764363510413855 ) ) ;
#2271 = CARTESIAN_POINT ( 'NONE',  ( 6.774437128121542528, -14.04910375689483537, -1.424172483101618036 ) ) ;
#2272 = ORIENTED_EDGE ( 'NONE', *, *, #13752, .T. ) ;
#2273 = CARTESIAN_POINT ( 'NONE',  ( 2.481649420246391902, 28.37819992234355126, 0.8687765177875720335 ) ) ;
#2274 = CARTESIAN_POINT ( 'NONE',  ( 4.730628863548789710E-15, -20.43486117963853843, -13.44550641761443366 ) ) ;
#2275 = CARTESIAN_POINT ( 'NONE',  ( -2.798362969681365886, 22.74680007765648071, 2.102939460078824929 ) ) ;
#2276 = VECTOR ( 'NONE', #5678, 1000.000000000000000 ) ;
#2277 = LINE ( 'NONE', #12077, #418 ) ;
#2278 = CIRCLE ( 'NONE', #9357, 6.000000000000000888 ) ;
#2279 = CARTESIAN_POINT ( 'NONE',  ( 4.243569643750003451, -23.29141514481821318, -13.25359815749571268 ) ) ;
#2280 = EDGE_CURVE ( 'NONE', #14538, #16354, #5427, .T. ) ;
#2281 = CYLINDRICAL_SURFACE ( 'NONE', #8778, 4.000000000000000000 ) ;
#2282 = CARTESIAN_POINT ( 'NONE',  ( -2.733110507866247652, 20.12180007765647716, 3.862833514489154574 ) ) ;
#2283 = CARTESIAN_POINT ( 'NONE',  ( 8.500000000000019540, 10.00000000000000000, -18.49999999999998934 ) ) ;
#2284 = DIRECTION ( 'NONE',  ( -0.000000000000000000, -0.5735764363510414965, -0.8191520442889950182 ) ) ;
#2285 = VECTOR ( 'NONE', #1273, 1000.000000000000000 ) ;
#2286 = CARTESIAN_POINT ( 'NONE',  ( 4.730628863548789710E-15, -18.88620480149072378, -11.23379589803414902 ) ) ;
#2287 = ORIENTED_EDGE ( 'NONE', *, *, #3935, .F. ) ;
#2288 = DIRECTION ( 'NONE',  ( -0.000000000000000000, -1.000000000000000000, -0.000000000000000000 ) ) ;
#2289 = CYLINDRICAL_SURFACE ( 'NONE', #8855, 4.000000000000000000 ) ;
#2290 = CARTESIAN_POINT ( 'NONE',  ( 0.7188294034286049072, 31.24680007765648071, -2.395093729190366005 ) ) ;
#2291 = ORIENTED_EDGE ( 'NONE', *, *, #16828, .T. ) ;
#2292 = CARTESIAN_POINT ( 'NONE',  ( 2.115076519116362963, 26.37180007765648071, -3.012182706137107591 ) ) ;
#2293 = CARTESIAN_POINT ( 'NONE',  ( -4.000000000000004441, -28.49678844617752205, -12.38983364346077565 ) ) ;
#2294 = CARTESIAN_POINT ( 'NONE',  ( 8.000000000000000000, 43.00000000000000000, 2.500000000000000000 ) ) ;
#2295 = ORIENTED_EDGE ( 'NONE', *, *, #15819, .F. ) ;
#2296 = CARTESIAN_POINT ( 'NONE',  ( 4.243569643750003451, -20.96843057759648943, -9.936032378125284836 ) ) ;
#2297 = CARTESIAN_POINT ( 'NONE',  ( 2.798362969681366330, 23.99680007765647716, -2.102939460078824929 ) ) ;
#2298 = CIRCLE ( 'NONE', #9082, 2.149999999999999023 ) ;
#2299 = EDGE_LOOP ( 'NONE', ( #9471, #2364, #2750, #3687 ) ) ;
#2300 = CARTESIAN_POINT ( 'NONE',  ( -5.577813053751546416E-15, -29.51599103134483570, -10.89793650852800511 ) ) ;
#2301 = CARTESIAN_POINT ( 'NONE',  ( 1.533898589781675205E-14, -27.51564321027552040, -8.041143755076902266 ) ) ;
#2302 = CARTESIAN_POINT ( 'NONE',  ( -3.658469487637143303, -25.65435779525035898, -15.39514208652095029 ) ) ;
#2303 = CARTESIAN_POINT ( 'NONE',  ( 7.076300148717182381, -12.11289111431826448, 11.47713140425214284 ) ) ;
#2304 = CARTESIAN_POINT ( 'NONE',  ( 0.000000000000000000, 18.79999999999999361, 2.500000000000000000 ) ) ;
#2305 = CARTESIAN_POINT ( 'NONE',  ( 4.243569643750003451, -25.06591724477924288, -15.78784979451479309 ) ) ;
#2306 = ADVANCED_FACE ( 'NONE', ( #1880 ), #14577, .F. ) ;
#2307 = VERTEX_POINT ( 'NONE', #4736 ) ;
#2308 = CARTESIAN_POINT ( 'NONE',  ( 8.000000000000000000, 7.960204194457795477E-16, -6.500000000000000000 ) ) ;
#2309 = CARTESIAN_POINT ( 'NONE',  ( 4.000000000000003553, -20.71259157640914239, -9.325484213969829739 ) ) ;
#2310 = CIRCLE ( 'NONE', #12648, 2.200000000000000622 ) ;
#2311 = CARTESIAN_POINT ( 'NONE',  ( -3.500000000000000444, 32.99680007765648071, 0.05647727720536892260 ) ) ;
#2312 = ADVANCED_FACE ( 'NONE', ( #7695 ), #13356, .F. ) ;
#2313 = ORIENTED_EDGE ( 'NONE', *, *, #7031, .F. ) ;
#2314 = VECTOR ( 'NONE', #15723, 1000.000000000000000 ) ;
#2315 = VERTEX_POINT ( 'NONE', #15970 ) ;
#2316 = DIRECTION ( 'NONE',  ( 0.000000000000000000, 0.000000000000000000, -1.000000000000000000 ) ) ;
#2317 = ADVANCED_FACE ( 'NONE', ( #13074 ), #12223, .T. ) ;
#2318 = CARTESIAN_POINT ( 'NONE',  ( 4.481649420246397675, 30.87819992234354061, 1.518615910253363177 ) ) ;
#2319 = CARTESIAN_POINT ( 'NONE',  ( 0.05938372350920110426, 35.12819992234354771, -3.680117784833935701 ) ) ;
#2320 = CARTESIAN_POINT ( 'NONE',  ( -1.593127413382952939, 29.12819992234354416, 2.091722143975172532 ) ) ;
#2321 = ORIENTED_EDGE ( 'NONE', *, *, #5925, .T. ) ;
#2322 = ADVANCED_FACE ( 'NONE', ( #1785 ), #390, .F. ) ;
#2323 = CARTESIAN_POINT ( 'NONE',  ( -3.673772985318219053, 28.24680007765647360, -2.599342558260952174 ) ) ;
#2324 = CARTESIAN_POINT ( 'NONE',  ( -1.999999999999996225, -18.08900519282243025, -7.591773503273958390 ) ) ;
#2325 = ORIENTED_EDGE ( 'NONE', *, *, #16764, .T. ) ;
#2326 = COLOUR_RGB ( '',0.8941176470588234615, 0.8941176470588234615, 0.8941176470588234615 ) ;
#2327 = CARTESIAN_POINT ( 'NONE',  ( -1.071796769724505882, -18.43433354004959668, -9.019263815904585257 ) ) ;
#2328 = CIRCLE ( 'NONE', #7927, 2.000000000000001776 ) ;
#2329 = CARTESIAN_POINT ( 'NONE',  ( -9.000000000000001776, 31.99999999999999289, 2.499999999999998224 ) ) ;
#2330 = ADVANCED_FACE ( 'NONE', ( #10287 ), #16988, .T. ) ;
#2331 = LINE ( 'NONE', #12225, #8909 ) ;
#2332 = CARTESIAN_POINT ( 'NONE',  ( 2.121784821875004390, -17.33009188869154826, -6.875691287533610918 ) ) ;
#2333 = CARTESIAN_POINT ( 'NONE',  ( 4.730628863548789710E-15, -20.72523425054125212, -13.86020214003574047 ) ) ;
#2334 = PRODUCT_DEFINITION ( 'UNKNOWN', '', #8054, #8397 ) ;
#2335 = DIRECTION ( 'NONE',  ( -0.000000000000000000, -0.5735764363510414965, -0.8191520442889950182 ) ) ;
#2336 = EDGE_LOOP ( 'NONE', ( #2937, #8500, #14384, #14550 ) ) ;
#2337 = CARTESIAN_POINT ( 'NONE',  ( 0.9009846993710122209, -10.00000000000000178, 24.02174733379527538 ) ) ;
#2338 =( LENGTH_UNIT ( ) NAMED_UNIT ( * ) SI_UNIT ( .MILLI., .METRE. ) );
#2339 = PRODUCT_DEFINITION_SHAPE ( 'NONE', 'NONE',  #18379 ) ;
#2340 = FILL_AREA_STYLE ('',( #9274 ) ) ;
#2341 = CARTESIAN_POINT ( 'NONE',  ( 4.243569643750003451, -24.32385273025008843, -14.72807183721590718 ) ) ;
#2342 = VERTEX_POINT ( 'NONE', #7514 ) ;
#2343 = AXIS2_PLACEMENT_3D ( 'NONE', #16824, #4098, #9748 ) ;
#2344 = CARTESIAN_POINT ( 'NONE',  ( 2.115076519116426024, 33.62819992234353350, 3.012182706137062294 ) ) ;
#2345 = DIRECTION ( 'NONE',  ( -1.000000000000000000, 0.000000000000000000, 4.336808689942021680E-16 ) ) ;
#2346 = CIRCLE ( 'NONE', #8821, 7.500000000000000888 ) ;
#2347 = CARTESIAN_POINT ( 'NONE',  ( 4.243569643749996345, -22.41197890986777352, -3.454652828211636884 ) ) ;
#2348 = CARTESIAN_POINT ( 'NONE',  ( -0.05938372350926768989, 28.62180007765647716, -2.628655560595669183 ) ) ;
#2349 = CARTESIAN_POINT ( 'NONE',  ( -4.481649420246396787, 19.62819992234354416, -1.518615910253363399 ) ) ;
#2350 = CARTESIAN_POINT ( 'NONE',  ( 1.999999999999994449, -27.50684327934278528, -8.962886473122447129 ) ) ;
#2351 =( BOUNDED_CURVE ( )  B_SPLINE_CURVE ( 2, ( #10903, #1000, #4036, #1357, #18341, #15460, #1272, #12381, #16946, #18250, #5614, #15093, #12289, #6819, #8026, #6641, #16581, #5521, #9506, #15184, #13777, #11079, #10993, #1089, #18071, #5341, #16765, #9685, #15368, #3950, #15275, #2576, #8208, #2668, #13872, #8302, #15909, #11432, #1628, #5706, #49, #8469, #3019, #1818, #12748, #14139, #17220, #3205, #7455, #17318, #14420, #1539, #11714, #1724, #4582, #6062, #7083, #14329, #5970, #15542, #9867, #13113, #10228, #15628, #17410, #7262, #5789, #425, #2839, #8842, #12921, #233, #5880, #11623, #1451, #7357, #9954, #11529, #11346, #17036, #14520, #4306, #8745, #17123, #8652, #2927, #4493, #8563, #12835, #138, #4401, #10135, #3113, #14236, #7175, #10042, #15719, #15815, #13019, #332, #17508, #6684, #15239, #10422, #13828, #7730, #7546, #12432, #10951, #13390, #4769, #10514, #3813, #16183, #10324, #5300, #2009, #16635, #2534, #17601, #16102, #11904, #3479, #16536, #9125, #3392, #18025, #7636, #8164, #1045, #703, #2445, #14803, #13301, #517, #2102, #5207, #14617, #6599, #8938, #12246, #13201, #613, #1137, #11810, #17934, #10858, #1919, #12337, #9467, #3908, #4675, #9560, #6161, #6774, #15139, #8076, #9032, #13735, #14710, #6253, #4864, #16005, #3297, #2886, #8431, #14008, #12701, #4353, #5567, #16996, #11216, #5392, #98, #15420, #5753, #15681, #12610, #5482, #7038, #18299, #11303, #16905, #16814, #12793, #2715, #10003, #14192, #2802, #15584, #4180, #8350, #13923, #9826, #8, #9644, #15506, #4000, #14098, #9738, #1410, #8606, #6866, #5659, #4270, #15323, #1495, #9913, #7130, #7222, #11390, #8264, #2976, #8518, #17081, #18214, #14285, #12522, #2623, #1588, #18123, #11042, #1232, #11128, #16725, #4084, #1320, #6954, #11577, #14477, #2059, #4728, #3159, #10377, #8995, #10088, #4630, #15862, #14670, #12878, #10279, #185, #5835, #3349, #17556, #17178, #17271, #383, #14571, #17365, #8894, #13160, #4826, #11482, #4451, #6021, #15768, #571, #11672, #14761, #16056, #3067, #6213, #1779, #15961, #8700, #14374, #7409, #5930, #3255, #470, #1873, #3441, #4543, #1676, #11765, #13067, #7504, #10185, #6114, #8796, #17459, #7311, #1967, #12971, #7593, #13252, #287, #11861, #10473, #16150, #9081, #6484, #17738, #5089, #6665, #15118, #13713, #12043, #8051, #932, #843, #9444, #15214, #2422, #16238, #18005, #12133, #17826, #7783, #6574, #14856, #10562, #12315, #2332, #1025, #10930, #11958, #13440, #17913, #661, #3530, #17651, #15028, #5276, #16613, #3886, #12226, #5001, #9535, #5182, #7690, #13351, #4910, #10749, #3791, #6308, #9177, #16512, #2151, #753, #6398, #16422, #3616, #10658, #16329, #9266, #3704, #9352 ),
 .UNSPECIFIED., .F., .F. ) 
 B_SPLINE_CURVE_WITH_KNOTS ( ( 3, 2, 2, 2, 2, 2, 2, 2, 2, 2, 2, 2, 2, 2, 2, 2, 2, 2, 2, 2, 2, 2, 2, 2, 2, 2, 2, 2, 2, 2, 2, 2, 2, 2, 2, 2, 2, 2, 2, 2, 2, 2, 2, 2, 2, 2, 2, 2, 2, 2, 2, 2, 2, 2, 2, 2, 2, 2, 2, 2, 2, 2, 2, 2, 2, 2, 2, 2, 2, 2, 2, 2, 2, 2, 2, 2, 2, 2, 2, 2, 2, 2, 2, 2, 2, 2, 2, 2, 2, 2, 2, 2, 2, 2, 2, 2, 2, 2, 2, 2, 2, 2, 2, 2, 2, 2, 2, 2, 2, 2, 2, 2, 2, 2, 2, 2, 2, 2, 2, 2, 2, 2, 2, 2, 2, 2, 2, 2, 2, 2, 2, 2, 2, 2, 2, 2, 2, 2, 2, 2, 2, 2, 2, 2, 2, 2, 2, 2, 2, 2, 2, 2, 2, 2, 2, 2, 2, 2, 2, 2, 2, 2, 2, 2, 2, 2, 2, 2, 2, 2, 2, 2, 2, 2, 3 ),
 ( 0.000000000000000000, 0.005769117253040331565, 0.01153823450608066313, 0.01730735175912099383, 0.02307646901216132626, 0.02884558626520165869, 0.03461470351824198766, 0.04038382077128232356, 0.04615293802432265252, 0.05192205527736298148, 0.05769117253040331739, 0.06346028978344366023, 0.06922940703648397531, 0.07499852428952431815, 0.08076764154256464712, 0.08653675879560497608, 0.09230587604864530504, 0.09807499330168564788, 0.1038441105547259630, 0.1096132278077663058, 0.1153823450608066348, 0.1211514623138469637, 0.1269205795668873205, 0.1326896968199276217, 0.1384588140729679506, 0.1442279313260082796, 0.1499970485790486363, 0.1557661658320889653, 0.1615352830851292942, 0.1673044003381695954, 0.1730735175912099522, 0.1788426348442502811, 0.1846117520972906101, 0.1903808693503309390, 0.1961499866033712958, 0.2019191038564116247, 0.2076882211094519259, 0.2134573383624922549, 0.2192264556155326116, 0.2249955728685729406, 0.2307646901216132695, 0.2365338073746535985, 0.2423029246276939275, 0.2480720418807342564, 0.2538411591337746409, 0.2596102763868149421, 0.2653793936398552433, 0.2711485108928956000, 0.2769176281459359013, 0.2826867453989762580, 0.2884558626520165592, 0.2942249799050568604, 0.2999940971580972726, 0.3057632144111375738, 0.3115323316641779305, 0.3173014489172182317, 0.3230705661702585885, 0.3288396834232988897, 0.3346088006763391909, 0.3403779179293795476, 0.3461470351824199043, 0.3519161524354602610, 0.3576852696885005622, 0.3634543869415409190, 0.3692235041945812202, 0.3749926214476215214, 0.3807617387006618781, 0.3865308559537021793, 0.3922999732067425915, 0.3980690904597828927, 0.4038382077128232495, 0.4096073249658635507, 0.4153764422189038519, 0.4211455594719442086, 0.4269146767249845098, 0.4326837939780248665, 0.4384529112310652232, 0.4442220284841055244, 0.4499911457371458812, 0.4557602629901861824, 0.4615293802432265391, 0.4672984974962668403, 0.4730676147493071970, 0.4788367320023474982, 0.4846058492553878549, 0.4903749665084282117, 0.4961440837614685129, 0.5019132010145088696, 0.5076823182675492818, 0.5134514355205894720, 0.5192205527736298842, 0.5249896700266701854, 0.5307587872797104867, 0.5365279045327507879, 0.5422970217857912001, 0.5480661390388316123, 0.5538352562918718025, 0.5596043735449122147, 0.5653734907979525159, 0.5711426080509928171, 0.5769117253040331184, 0.5826808425570735306, 0.5884499598101137208, 0.5942190770631541330, 0.5999881943161945452, 0.6057573115692348464, 0.6115264288222751476, 0.6172955460753154489, 0.6230646633283558611, 0.6288337805813960513, 0.6346028978344364635, 0.6403720150874768757, 0.6461411323405171769, 0.6519102495935574781, 0.6576793668465977794, 0.6634484840996381916, 0.6692176013526783818, 0.6749867186057187940, 0.6807558358587590952, 0.6865249531117995074, 0.6922940703648398086, 0.6980631876178801098, 0.7038323048709205221, 0.7096014221239607123, 0.7153705393770011245, 0.7211396566300414257, 0.7269087738830818379, 0.7326778911361221391, 0.7384470083891624403, 0.7442161256422028526, 0.7499852428952430428, 0.7557543601482834550, 0.7615234774013237562, 0.7672925946543641684, 0.7730617119074043586, 0.7788308291604447708, 0.7845999464134851831, 0.7903690636665253733, 0.7961381809195657855, 0.8019072981726060867, 0.8076764154256464989, 0.8134455326786866891, 0.8192146499317271013, 0.8249837671847675136, 0.8307528844378077038, 0.8365220016908481160, 0.8422911189438884172, 0.8480602361969287184, 0.8538293534499690196, 0.8595984707030094318, 0.8653675879560497330, 0.8711367052090900343, 0.8769058224621304465, 0.8826749397151707477, 0.8884440569682110489, 0.8942131742212513501, 0.8999822914742917623, 0.9057514087273320635, 0.9115205259803723647, 0.9172896432334127770, 0.9230587604864530782, 0.9288278777394933794, 0.9345969949925336806, 0.9403661122455740928, 0.9461352294986143940, 0.9519043467516546952, 0.9576734640046949965, 0.9634425812577354087, 0.9692116985107757099, 0.9749808157638160111, 0.9807499330168564233, 0.9865190502698967245, 0.9922881675229370257, 0.9980572847759773270, 1.000000000000000000 ),
 .UNSPECIFIED. ) 
 CURVE ( )  GEOMETRIC_REPRESENTATION_ITEM ( )  RATIONAL_B_SPLINE_CURVE ( ( 1.000000000000000000, 0.8660254037844387076, 1.000000000000000000, 0.8660254037844387076, 1.000000000000000000, 0.8660254037844387076, 1.000000000000000000, 0.8660254037844387076, 1.000000000000000000, 0.8660254037844387076, 1.000000000000000000, 0.8660254037844387076, 1.000000000000000000, 0.8660254037844387076, 1.000000000000000000, 0.8660254037844387076, 1.000000000000000000, 0.8660254037844387076, 1.000000000000000000, 0.8660254037844387076, 1.000000000000000000, 0.8660254037844387076, 1.000000000000000000, 0.8660254037844387076, 1.000000000000000000, 0.8660254037844387076, 1.000000000000000000, 0.8660254037844387076, 1.000000000000000000, 0.8660254037844387076, 1.000000000000000000, 0.8660254037844387076, 1.000000000000000000, 0.8660254037844387076, 1.000000000000000000, 0.8660254037844387076, 1.000000000000000000, 0.8660254037844387076, 1.000000000000000000, 0.8660254037844387076, 1.000000000000000000, 0.8660254037844387076, 1.000000000000000000, 0.8660254037844387076, 1.000000000000000000, 0.8660254037844387076, 1.000000000000000000, 0.8660254037844387076, 1.000000000000000000, 0.8660254037844387076, 1.000000000000000000, 0.8660254037844387076, 1.000000000000000000, 0.8660254037844387076, 1.000000000000000000, 0.8660254037844387076, 1.000000000000000000, 0.8660254037844387076, 1.000000000000000000, 0.8660254037844387076, 1.000000000000000000, 0.8660254037844387076, 1.000000000000000000, 0.8660254037844387076, 1.000000000000000000, 0.8660254037844387076, 1.000000000000000000, 0.8660254037844387076, 1.000000000000000000, 0.8660254037844387076, 1.000000000000000000, 0.8660254037844387076, 1.000000000000000000, 0.8660254037844387076, 1.000000000000000000, 0.8660254037844387076, 1.000000000000000000, 0.8660254037844387076, 1.000000000000000000, 0.8660254037844387076, 1.000000000000000000, 0.8660254037844387076, 1.000000000000000000, 0.8660254037844387076, 1.000000000000000000, 0.8660254037844387076, 1.000000000000000000, 0.8660254037844387076, 1.000000000000000000, 0.8660254037844387076, 1.000000000000000000, 0.8660254037844387076, 1.000000000000000000, 0.8660254037844387076, 1.000000000000000000, 0.8660254037844387076, 1.000000000000000000, 0.8660254037844387076, 1.000000000000000000, 0.8660254037844387076, 1.000000000000000000, 0.8660254037844387076, 1.000000000000000000, 0.8660254037844387076, 1.000000000000000000, 0.8660254037844387076, 1.000000000000000000, 0.8660254037844387076, 1.000000000000000000, 0.8660254037844387076, 1.000000000000000000, 0.8660254037844387076, 1.000000000000000000, 0.8660254037844387076, 1.000000000000000000, 0.8660254037844387076, 1.000000000000000000, 0.8660254037844387076, 1.000000000000000000, 0.8660254037844387076, 1.000000000000000000, 0.8660254037844387076, 1.000000000000000000, 0.8660254037844387076, 1.000000000000000000, 0.8660254037844387076, 1.000000000000000000, 0.8660254037844387076, 1.000000000000000000, 0.8660254037844387076, 1.000000000000000000, 0.8660254037844387076, 1.000000000000000000, 0.8660254037844387076, 1.000000000000000000, 0.8660254037844387076, 1.000000000000000000, 0.8660254037844387076, 1.000000000000000000, 0.8660254037844387076, 1.000000000000000000, 0.8660254037844387076, 1.000000000000000000, 0.8660254037844387076, 1.000000000000000000, 0.8660254037844387076, 1.000000000000000000, 0.8660254037844387076, 1.000000000000000000, 0.8660254037844387076, 1.000000000000000000, 0.8660254037844387076, 1.000000000000000000, 0.8660254037844387076, 1.000000000000000000, 0.8660254037844387076, 1.000000000000000000, 0.8660254037844387076, 1.000000000000000000, 0.8660254037844387076, 1.000000000000000000, 0.8660254037844387076, 1.000000000000000000, 0.8660254037844387076, 1.000000000000000000, 0.8660254037844387076, 1.000000000000000000, 0.8660254037844387076, 1.000000000000000000, 0.8660254037844387076, 1.000000000000000000, 0.8660254037844387076, 1.000000000000000000, 0.8660254037844387076, 1.000000000000000000, 0.8660254037844387076, 1.000000000000000000, 0.8660254037844387076, 1.000000000000000000, 0.8660254037844387076, 1.000000000000000000, 0.8660254037844387076, 1.000000000000000000, 0.8660254037844387076, 1.000000000000000000, 0.8660254037844387076, 1.000000000000000000, 0.8660254037844387076, 1.000000000000000000, 0.8660254037844387076, 1.000000000000000000, 0.8660254037844387076, 1.000000000000000000, 0.8660254037844387076, 1.000000000000000000, 0.8660254037844387076, 1.000000000000000000, 0.8660254037844387076, 1.000000000000000000, 0.8660254037844387076, 1.000000000000000000, 0.8660254037844387076, 1.000000000000000000, 0.8660254037844387076, 1.000000000000000000, 0.8660254037844387076, 1.000000000000000000, 0.8660254037844387076, 1.000000000000000000, 0.8660254037844387076, 1.000000000000000000, 0.8660254037844387076, 1.000000000000000000, 0.8660254037844387076, 1.000000000000000000, 0.8660254037844387076, 1.000000000000000000, 0.8660254037844387076, 1.000000000000000000, 0.8660254037844387076, 1.000000000000000000, 0.8660254037844387076, 1.000000000000000000, 0.8660254037844387076, 1.000000000000000000, 0.8660254037844387076, 1.000000000000000000, 0.8660254037844387076, 1.000000000000000000, 0.8660254037844387076, 1.000000000000000000, 0.8660254037844387076, 1.000000000000000000, 0.8660254037844387076, 1.000000000000000000, 0.8660254037844387076, 1.000000000000000000, 0.8660254037844387076, 1.000000000000000000, 0.8660254037844387076, 1.000000000000000000, 0.8660254037844387076, 1.000000000000000000, 0.8660254037844387076, 1.000000000000000000, 0.8660254037844387076, 1.000000000000000000, 0.8660254037844387076, 1.000000000000000000, 0.8660254037844387076, 1.000000000000000000, 0.8660254037844387076, 1.000000000000000000, 0.8660254037844387076, 1.000000000000000000, 0.8660254037844387076, 1.000000000000000000, 0.8660254037844387076, 1.000000000000000000, 0.8660254037844387076, 1.000000000000000000, 0.8660254037844387076, 1.000000000000000000, 0.8660254037844387076, 1.000000000000000000, 0.8660254037844387076, 1.000000000000000000, 0.8660254037844387076, 1.000000000000000000, 0.8660254037844387076, 1.000000000000000000, 0.8660254037844387076, 1.000000000000000000, 0.8660254037844387076, 1.000000000000000000, 0.8660254037844387076, 1.000000000000000000, 0.8660254037844387076, 1.000000000000000000, 0.8660254037844387076, 1.000000000000000000, 0.8660254037844387076, 1.000000000000000000, 0.8660254037844387076, 1.000000000000000000, 0.8660254037844387076, 1.000000000000000000, 0.8660254037844387076, 1.000000000000000000, 0.8660254037844387076, 1.000000000000000000, 0.8660254037844387076, 1.000000000000000000, 0.8660254037844387076, 1.000000000000000000, 0.8660254037844387076, 1.000000000000000000, 0.8660254037844387076, 1.000000000000000000, 0.8660254037844387076, 1.000000000000000000, 0.8660254037844387076, 1.000000000000000000, 0.8660254037844387076, 1.000000000000000000, 0.8660254037844387076, 1.000000000000000000, 0.8660254037844387076, 1.000000000000000000, 0.8660254037844387076, 1.000000000000000000, 0.8660254037844387076, 1.000000000000000000, 0.8660254037844387076, 1.000000000000000000, 0.8660254037844387076, 1.000000000000000000, 0.8660254037844387076, 1.000000000000000000, 0.8660254037844387076, 1.000000000000000000, 0.8660254037844387076, 1.000000000000000000, 0.8660254037844387076, 1.000000000000000000, 0.8660254037844387076, 1.000000000000000000, 0.8660254037844387076, 1.000000000000000000, 0.8660254037844387076, 1.000000000000000000, 0.8660254037844387076, 1.000000000000000000, 0.8660254037844387076, 1.000000000000000000, 0.8660254037844387076, 1.000000000000000000, 0.8660254037844387076, 1.000000000000000000, 0.8660254037844387076, 1.000000000000000000, 0.8660254037844387076, 1.000000000000000000, 0.8660254037844387076, 1.000000000000000000, 0.8660254037844387076, 1.000000000000000000, 0.9548848677736452295, 0.9401542295229485813 ) ) 
 REPRESENTATION_ITEM ( '' )  );
#2352 = ORIENTED_EDGE ( 'NONE', *, *, #3438, .F. ) ;
#2353 = CARTESIAN_POINT ( 'NONE',  ( -2.121784821874996396, -16.80311853779403108, -6.123095346843099307 ) ) ;
#2354 = CARTESIAN_POINT ( 'NONE',  ( -1.027846397803541700, 17.49680007765647716, 3.346150245485522312 ) ) ;
#2355 = VECTOR ( 'NONE', #13808, 1000.000000000000000 ) ;
#2356 = DIRECTION ( 'NONE',  ( -3.373073425510457965E-16, 0.000000000000000000, -1.000000000000000000 ) ) ;
#2357 = CARTESIAN_POINT ( 'NONE',  ( 0.000000000000000000, 5.000000000000000000, 0.000000000000000000 ) ) ;
#2358 = CARTESIAN_POINT ( 'NONE',  ( -9.000000000000001776, 16.59999999999999787, 2.499999999999995559 ) ) ;
#2359 = ORIENTED_EDGE ( 'NONE', *, *, #16187, .F. ) ;
#2360 = ORIENTED_EDGE ( 'NONE', *, *, #12355, .F. ) ;
#2361 = CARTESIAN_POINT ( 'NONE',  ( -3.481649420246369697, 17.87180007765648071, 1.193696214020542490 ) ) ;
#2362 = CARTESIAN_POINT ( 'NONE',  ( -9.000000000000003553, 23.19999999999999574, -2.500000000000001776 ) ) ;
#2363 = DIRECTION ( 'NONE',  ( 3.469446951953612217E-16, -0.000000000000000000, 1.000000000000000000 ) ) ;
#2364 = ORIENTED_EDGE ( 'NONE', *, *, #5369, .F. ) ;
#2365 = CARTESIAN_POINT ( 'NONE',  ( -3.481649420246394122, 14.62819992234354061, -1.193696214020467883 ) ) ;
#2366 =( NAMED_UNIT ( * ) PLANE_ANGLE_UNIT ( ) SI_UNIT ( $, .RADIAN. ) );
#2367 = CARTESIAN_POINT ( 'NONE',  ( -2.121784821875005722, -27.86783793146007326, -9.110681959144070419 ) ) ;
#2368 = CARTESIAN_POINT ( 'NONE',  ( -2.211161402132902243, 28.37180007765647716, -2.942372952327172886 ) ) ;
#2369 = PRODUCT ( 'Plunger', 'Plunger', '', ( #14722 ) ) ;
#2370 = AXIS2_PLACEMENT_3D ( 'NONE', #16701, #4061, #13897 ) ;
#2371 = CARTESIAN_POINT ( 'NONE',  ( 9.000000000000001776, 18.79999999999999361, -2.500000000000002665 ) ) ;
#2372 = CIRCLE ( 'NONE', #13591, 8.000000000000003553 ) ;
#2373 = DIRECTION ( 'NONE',  ( -0.000000000000000000, -1.000000000000000000, -0.000000000000000000 ) ) ;
#2374 = CARTESIAN_POINT ( 'NONE',  ( 4.243569643750003451, -23.54952454117618288, -13.62221657742576397 ) ) ;
#2375 = CARTESIAN_POINT ( 'NONE',  ( 0.000000000000000000, 13.00000000000000178, 0.000000000000000000 ) ) ;
#2376 = CARTESIAN_POINT ( 'NONE',  ( 2.829195390882805583, 24.62180007765647716, 3.793023760679204770 ) ) ;
#2377 = CARTESIAN_POINT ( 'NONE',  ( -1.734723475976807094E-15, 27.59999999999999432, -11.50000000000000178 ) ) ;
#2378 = CARTESIAN_POINT ( 'NONE',  ( 0.000000000000000000, 15.00000000000000178, 0.000000000000000000 ) ) ;
#2379 = CARTESIAN_POINT ( 'NONE',  ( 4.243569643749996345, -23.44441649529964877, -4.929126507931827383 ) ) ;
#2380 = CARTESIAN_POINT ( 'NONE',  ( -1.071796769724505882, -18.75697028620200868, -9.480036841823904936 ) ) ;
#2381 = FACE_OUTER_BOUND ( 'NONE', #14338, .T. ) ;
#2382 = CARTESIAN_POINT ( 'NONE',  ( -1.593127413382998459, 35.87180007765648071, -2.091722143975139669 ) ) ;
#2383 = EDGE_CURVE ( 'NONE', #10239, #2662, #17878, .T. ) ;
#2384 = CARTESIAN_POINT ( 'NONE',  ( 1.071796769724494780, -26.72978832048277553, -6.918826660630844394 ) ) ;
#2385 = CARTESIAN_POINT ( 'NONE',  ( 1.135272562821090458, 32.24680007765648071, 3.311245368580554072 ) ) ;
#2386 = FACE_OUTER_BOUND ( 'NONE', #1173, .T. ) ;
#2387 = APPLICATION_PROTOCOL_DEFINITION ( 'draft international standard', 'automotive_design', 1998, #9141 ) ;
#2388 = CARTESIAN_POINT ( 'NONE',  ( -2.465190328815646976E-33, -26.97786251599082519, -14.24690051095425858 ) ) ;
#2389 = ORIENTED_EDGE ( 'NONE', *, *, #4375, .F. ) ;
#2390 = CARTESIAN_POINT ( 'NONE',  ( -4.243569643750000786, -21.31917248646755070, -6.165453624519022569 ) ) ;
#2391 = AXIS2_PLACEMENT_3D ( 'NONE', #5326, #8372, #11242 ) ;
#2392 = CARTESIAN_POINT ( 'NONE',  ( 1.135272562821090458, 24.74680007765647716, 3.311245368580554072 ) ) ;
#2393 = ORIENTED_EDGE ( 'NONE', *, *, #15984, .F. ) ;
#2394 = CARTESIAN_POINT ( 'NONE',  ( 1.999999999999994449, -24.66763991940512568, -4.908083853891920256 ) ) ;
#2395 = DIRECTION ( 'NONE',  ( 0.000000000000000000, 0.000000000000000000, 1.000000000000000000 ) ) ;
#2396 = CARTESIAN_POINT ( 'NONE',  ( 2.446180570232387108, -24.42336006072196142, -16.36676630457531445 ) ) ;
#2397 = CARTESIAN_POINT ( 'NONE',  ( 7.315923705238545516, -13.46616490046861792, 2.115434428656500998 ) ) ;
#2398 = CARTESIAN_POINT ( 'NONE',  ( -1.734723475976807094E-15, 38.59999999999999432, -11.50000000000000178 ) ) ;
#2399 = CARTESIAN_POINT ( 'NONE',  ( -4.243569643750000786, -25.93287794636623644, -12.75450788076862452 ) ) ;
#2400 = EDGE_LOOP ( 'NONE', ( #262, #11099, #10817, #12696 ) ) ;
#2401 = CARTESIAN_POINT ( 'NONE',  ( 2.000000000000004441, -20.26142594620695192, -10.69431187202529010 ) ) ;
#2402 = CARTESIAN_POINT ( 'NONE',  ( 1.999999999999994449, -24.73216726919956443, -5.000238459881198416 ) ) ;
#2403 = VECTOR ( 'NONE', #17387, 1000.000000000000000 ) ;
#2404 = CARTESIAN_POINT ( 'NONE',  ( -3.481649420246369697, 35.37180007765648071, 1.193696214020542490 ) ) ;
#2405 = ORIENTED_EDGE ( 'NONE', *, *, #16786, .T. ) ;
#2406 = VERTEX_POINT ( 'NONE', #6313 ) ;
#2407 = CARTESIAN_POINT ( 'NONE',  ( 1.071796769724504328, -25.69735073505090384, -5.444352980910657003 ) ) ;
#2408 =( NAMED_UNIT ( * ) SI_UNIT ( $, .STERADIAN. ) SOLID_ANGLE_UNIT ( ) );
#2409 = CARTESIAN_POINT ( 'NONE',  ( 0.05938372350919016857, 32.62819992234354771, -4.731580009072201776 ) ) ;
#2410 = DIRECTION ( 'NONE',  ( 3.469446951953612217E-16, -0.000000000000000000, 1.000000000000000000 ) ) ;
#2411 = CARTESIAN_POINT ( 'NONE',  ( 0.7188294034286553114, 26.25319992234354416, 2.395093729190349130 ) ) ;
#2412 = VERTEX_POINT ( 'NONE', #10569 ) ;
#2413 = CARTESIAN_POINT ( 'NONE',  ( 4.481649420246366589, 29.12180007765647005, -1.518615910253458212 ) ) ;
#2414 = CARTESIAN_POINT ( 'NONE',  ( 4.713407268011036227E-15, -17.42274839898859895, -8.653419144721045342 ) ) ;
#2415 = ORIENTED_EDGE ( 'NONE', *, *, #14835, .F. ) ;
#2416 = EDGE_CURVE ( 'NONE', #904, #2199, #14614, .T. ) ;
#2417 = AXIS2_PLACEMENT_3D ( 'NONE', #6825, #14623, #14426 ) ;
#2418 = DIRECTION ( 'NONE',  ( 0.000000000000000000, 0.000000000000000000, -1.000000000000000000 ) ) ;
#2419 = EDGE_CURVE ( 'NONE', #3719, #17692, #11325, .T. ) ;
#2420 = CARTESIAN_POINT ( 'NONE',  ( -8.500000000000010658, 13.00000000000000000, 20.49999999999998934 ) ) ;
#2421 = DIRECTION ( 'NONE',  ( -0.000000000000000000, -1.000000000000000000, -0.000000000000000000 ) ) ;
#2422 = CARTESIAN_POINT ( 'NONE',  ( -2.121784821874996396, -17.54518305232318554, -7.182873304141986992 ) ) ;
#2423 = CARTESIAN_POINT ( 'NONE',  ( -4.243569643750000786, -23.90026645004723704, -9.851637823819498152 ) ) ;
#2424 = EDGE_CURVE ( 'NONE', #18219, #6378, #14862, .T. ) ;
#2425 = FACE_OUTER_BOUND ( 'NONE', #4834, .T. ) ;
#2426 = EDGE_LOOP ( 'NONE', ( #5914, #12294, #16787, #1295 ) ) ;
#2427 = MANIFOLD_SOLID_BREP ( 'Cavity1', #15632 ) ;
#2428 = CARTESIAN_POINT ( 'NONE',  ( -8.999999999999996447, -10.00000000000000000, -3.713574246709372417 ) ) ;
#2429 = CARTESIAN_POINT ( 'NONE',  ( 0.05938372350927906967, 17.37180007765647360, 3.680117784833935701 ) ) ;
#2430 = CARTESIAN_POINT ( 'NONE',  ( 9.184850993605147944E-16, -33.35093342269870931, -10.27273805603704737 ) ) ;
#2431 = VERTEX_POINT ( 'NONE', #16518 ) ;
#2432 = TOROIDAL_SURFACE ( 'NONE', #5066, 9.000000000000001776, 0.9999999999999991118 ) ;
#2433 = CARTESIAN_POINT ( 'NONE',  ( 2.211161402132839626, 35.37819992234353350, -2.942372952327218183 ) ) ;
#2434 = CARTESIAN_POINT ( 'NONE',  ( 1.027846397803612311, 18.75319992234354771, 3.346150245485499219 ) ) ;
#2435 = CARTESIAN_POINT ( 'NONE',  ( -2.121784821875005722, -22.96375940065866672, -2.106931980473163879 ) ) ;
#2436 = CARTESIAN_POINT ( 'NONE',  ( -0.7188294034286043521, 27.49680007765648071, 2.395093729190366005 ) ) ;
#2437 = CARTESIAN_POINT ( 'NONE',  ( -1.444289557195956863, 29.00319992234354771, 4.262301884875733471 ) ) ;
#2438 = CARTESIAN_POINT ( 'NONE',  ( 4.000000000000003553, -22.45483000112048799, -11.81365854749089017 ) ) ;
#2439 = VERTEX_POINT ( 'NONE', #16430 ) ;
#2440 = CARTESIAN_POINT ( 'NONE',  ( 4.243569643750003451, -17.87111782130087434, -5.512611338964712893 ) ) ;
#2441 = EDGE_CURVE ( 'NONE', #15144, #8682, #6404, .T. ) ;
#2442 = CARTESIAN_POINT ( 'NONE',  ( 3.673772985318219053, 39.49680007765648071, 2.599342558260951730 ) ) ;
#2443 = DIRECTION ( 'NONE',  ( -1.000000000000000000, 0.000000000000000000, 4.336808689942021680E-16 ) ) ;
#2444 = COLOUR_RGB ( '',0.8941176470588234615, 0.8941176470588234615, 0.8941176470588234615 ) ;
#2445 = CARTESIAN_POINT ( 'NONE',  ( 4.243569643749997233, -26.28361985523730837, -8.983929127162353367 ) ) ;
#2446 = CARTESIAN_POINT ( 'NONE',  ( -4.000000000000000888, -20.62550348340303685, -5.174791620453635943 ) ) ;
#2447 = DIRECTION ( 'NONE',  ( -1.000000000000000000, 0.000000000000000000, 0.000000000000000000 ) ) ;
#2448 = CARTESIAN_POINT ( 'NONE',  ( 0.000000000000000000, 5.977523610840987267, 32.81826849749789687 ) ) ;
#2449 = ORIENTED_EDGE ( 'NONE', *, *, #14993, .T. ) ;
#2450 = EDGE_LOOP ( 'NONE', ( #14044, #9156, #13004, #5784 ) ) ;
#2451 = CARTESIAN_POINT ( 'NONE',  ( 2.115076519116362963, 18.87180007765648071, -3.012182706137107147 ) ) ;
#2452 = DIRECTION ( 'NONE',  ( -1.000000000000000000, 0.000000000000000000, 0.000000000000000000 ) ) ;
#2453 = AXIS2_PLACEMENT_3D ( 'NONE', #14576, #8898, #389 ) ;
#2454 = CARTESIAN_POINT ( 'NONE',  ( 4.000000000000000000, 3.732111120401558708E-16, -3.047499999999999876 ) ) ;
#2455 = CARTESIAN_POINT ( 'NONE',  ( 1.999999999999994449, -26.99062448662684943, -8.225649633262349880 ) ) ;
#2456 = ORIENTED_EDGE ( 'NONE', *, *, #16482, .F. ) ;
#2457 = CARTESIAN_POINT ( 'NONE',  ( 1.989345975306457071, 33.50319992234354061, 1.515154207786300500 ) ) ;
#2458 = CARTESIAN_POINT ( 'NONE',  ( 2.121784821874994176, -27.30860090601781209, -8.312008715962296179 ) ) ;
#2459 = CARTESIAN_POINT ( 'NONE',  ( 0.05938372350927906274, 27.37180007765647716, 3.680117784833935701 ) ) ;
#2460 =( BOUNDED_CURVE ( )  B_SPLINE_CURVE ( 2, ( #7648, #530, #6266, #11919, #17616, #16295, #11728, #16200, #6177 ),
 .UNSPECIFIED., .F., .F. ) 
 B_SPLINE_CURVE_WITH_KNOTS ( ( 3, 2, 2, 2, 3 ),
 ( 0.8879310344827586743, 0.8908045977011493921, 0.8965517241379310498, 0.9022988505747125965, 0.9051724137931034253 ),
 .UNSPECIFIED. ) 
 CURVE ( )  GEOMETRIC_REPRESENTATION_ITEM ( )  RATIONAL_B_SPLINE_CURVE ( ( 0.9330127018922194093, 0.9330127018922206306, 1.000000000000000000, 0.8660254037844387076, 1.000000000000000000, 0.8660254037844387076, 1.000000000000000000, 0.9330127018922194093, 0.9330127018922194093 ) ) 
 REPRESENTATION_ITEM ( '' )  );
#2461 = FILL_AREA_STYLE_COLOUR ( '', #10696 ) ;
#2462 = CARTESIAN_POINT ( 'NONE',  ( -2.864755990943222308, 26.75319992234354771, 2.011557305968548093 ) ) ;
#2463 = EDGE_CURVE ( 'NONE', #9743, #17585, #13813, .T. ) ;
#2464 = CYLINDRICAL_SURFACE ( 'NONE', #16413, 4.000000000000000000 ) ;
#2465 = DIRECTION ( 'NONE',  ( -0.000000000000000000, -1.000000000000000000, -0.000000000000000000 ) ) ;
#2466 = CARTESIAN_POINT ( 'NONE',  ( 4.243569643749996345, -26.05777413342408622, -8.661388009723561154 ) ) ;
#2467 = DIRECTION ( 'NONE',  ( -0.000000000000000000, -1.000000000000000000, -0.000000000000000000 ) ) ;
#2468 = CARTESIAN_POINT ( 'NONE',  ( 4.518350579753633411, 19.37180007765647716, 1.405661355842698468 ) ) ;
#2469 = CARTESIAN_POINT ( 'NONE',  ( -8.500000000000010658, 15.00000000000000178, 18.34999999999999432 ) ) ;
#2470 = CYLINDRICAL_SURFACE ( 'NONE', #18321, 0.9999999999999991118 ) ;
#2471 = CARTESIAN_POINT ( 'NONE',  ( 4.243569643750000786, -22.44840109553366858, -7.778159211712977417 ) ) ;
#2472 = ORIENTED_EDGE ( 'NONE', *, *, #6638, .T. ) ;
#2473 = CARTESIAN_POINT ( 'NONE',  ( -4.648177544792955347E-16, -30.03220982406077155, -11.63517334838810058 ) ) ;
#2474 = DIRECTION ( 'NONE',  ( 0.000000000000000000, 0.000000000000000000, -1.000000000000000000 ) ) ;
#2475 = CARTESIAN_POINT ( 'NONE',  ( 0.7188294034286049072, 36.24680007765647360, -2.395093729190366005 ) ) ;
#2476 = CARTESIAN_POINT ( 'NONE',  ( 4.299564228933482956E-15, -16.63909446626264454, -6.455396711050170211 ) ) ;
#2477 = CARTESIAN_POINT ( 'NONE',  ( -3.518350579753630303, 35.62180007765648071, -1.080741659609802952 ) ) ;
#2478 = CARTESIAN_POINT ( 'NONE',  ( 10.00000000000000355, 40.79999999999999716, 2.499999999999996891 ) ) ;
#2479 = VECTOR ( 'NONE', #1789, 1000.000000000000000 ) ;
#2480 = CARTESIAN_POINT ( 'NONE',  ( -2.590630740757541073, 15.00000000000000888, -2.889634409359581380 ) ) ;
#2481 = ORIENTED_EDGE ( 'NONE', *, *, #6992, .T. ) ;
#2482 = CARTESIAN_POINT ( 'NONE',  ( -4.243569643750004339, -22.78838844622314497, -3.992221357276295901 ) ) ;
#2483 = EDGE_CURVE ( 'NONE', #10052, #11668, #1581, .T. ) ;
#2484 = CARTESIAN_POINT ( 'NONE',  ( 3.500000000000000444, 26.74680007765648071, -0.05647727720536935281 ) ) ;
#2485 = ORIENTED_EDGE ( 'NONE', *, *, #13294, .T. ) ;
#2486 = ADVANCED_FACE ( 'NONE', ( #18108 ), #12506, .F. ) ;
#2487 = DIRECTION ( 'NONE',  ( -1.000000000000000000, -0.000000000000000000, -0.000000000000000000 ) ) ;
#2488 = ADVANCED_FACE ( 'NONE', ( #18199 ), #14307, .T. ) ;
#2489 = DIRECTION ( 'NONE',  ( 0.000000000000000000, 0.000000000000000000, -1.000000000000000000 ) ) ;
#2490 = CARTESIAN_POINT ( 'NONE',  ( 9.999999999999998224, 40.79999999999999716, -2.500000000000001776 ) ) ;
#2491 = TOROIDAL_SURFACE ( 'NONE', #17297, 9.000000000000003553, 0.9999999999999991118 ) ;
#2492 = CARTESIAN_POINT ( 'NONE',  ( 8.673617379884035472E-15, 13.00000000000000178, 3.469446951953614189E-15 ) ) ;
#2493 = CARTESIAN_POINT ( 'NONE',  ( -5.330712181944245322E-15, -29.62412893858816076, -9.483180404412477671 ) ) ;
#2494 = EDGE_LOOP ( 'NONE', ( #9062, #15099 ) ) ;
#2495 = CARTESIAN_POINT ( 'NONE',  ( 9.999999999999998224, 31.99999999999999289, -2.500000000000001776 ) ) ;
#2496 = CARTESIAN_POINT ( 'NONE',  ( 4.713407268011036227E-15, -18.26160393785694325, -9.851429010500462269 ) ) ;
#2497 = CARTESIAN_POINT ( 'NONE',  ( -1.027846397803541700, 37.49680007765647360, 3.346150245485522312 ) ) ;
#2498 = ORIENTED_EDGE ( 'NONE', *, *, #17032, .F. ) ;
#2499 = ORIENTED_EDGE ( 'NONE', *, *, #9322, .F. ) ;
#2500 = DIRECTION ( 'NONE',  ( 0.000000000000000000, 0.000000000000000000, 1.000000000000000000 ) ) ;
#2501 = CARTESIAN_POINT ( 'NONE',  ( -1.444289557195956863, 36.50319992234354061, 4.262301884875733471 ) ) ;
#2502 = UNCERTAINTY_MEASURE_WITH_UNIT (LENGTH_MEASURE( 1.000000000000000082E-05 ), #4384, 'distance_accuracy_value', 'NONE');
#2503 = LINE ( 'NONE', #16686, #9260 ) ;
#2504 = CARTESIAN_POINT ( 'NONE',  ( 2.518350579753611207, 30.62819992234355126, -0.7558219633769606149 ) ) ;
#2505 = AXIS2_PLACEMENT_3D ( 'NONE', #10034, #3010, #8643 ) ;
#2506 = ORIENTED_EDGE ( 'NONE', *, *, #4378, .T. ) ;
#2507 = CARTESIAN_POINT ( 'NONE',  ( -4.243569643750000786, -25.44892282819504459, -12.06334834339978634 ) ) ;
#2508 = CARTESIAN_POINT ( 'NONE',  ( 1.444289557196047680, 24.74680007765647716, 4.262301884875704161 ) ) ;
#2509 = UNCERTAINTY_MEASURE_WITH_UNIT (LENGTH_MEASURE( 1.000000000000000082E-05 ), #16475, 'distance_accuracy_value', 'NONE');
#2510 = CARTESIAN_POINT ( 'NONE',  ( -4.000000000000004441, -21.97952618743386566, -3.082218539220304976 ) ) ;
#2511 = ORIENTED_EDGE ( 'NONE', *, *, #16394, .F. ) ;
#2512 = LINE ( 'NONE', #8140, #4717 ) ;
#2513 = CARTESIAN_POINT ( 'NONE',  ( -1.734723475976807094E-15, 18.79999999999999361, -2.500000000000000000 ) ) ;
#2514 = DIRECTION ( 'NONE',  ( -0.000000000000000000, -0.000000000000000000, 1.000000000000000000 ) ) ;
#2515 = DIRECTION ( 'NONE',  ( 0.000000000000000000, 0.000000000000000000, 1.000000000000000000 ) ) ;
#2516 = CARTESIAN_POINT ( 'NONE',  ( 4.243569643750003451, -20.45221178488055713, -9.198795538265191141 ) ) ;
#2517 = CARTESIAN_POINT ( 'NONE',  ( -3.291771655530798757, -28.93493258167780269, -13.02337503524261386 ) ) ;
#2518 = VERTEX_POINT ( 'NONE', #2249 ) ;
#2519 = CARTESIAN_POINT ( 'NONE',  ( -4.000000000000000888, -25.07789057128293919, -11.53345936525372650 ) ) ;
#2520 = CARTESIAN_POINT ( 'NONE',  ( 0.3999999999999975797, 0.000000000000000000, 0.000000000000000000 ) ) ;
#2521 = DIRECTION ( 'NONE',  ( 0.000000000000000000, 1.000000000000000000, 0.000000000000000000 ) ) ;
#2522 = ORIENTED_EDGE ( 'NONE', *, *, #12871, .T. ) ;
#2523 = CARTESIAN_POINT ( 'NONE',  ( -2.798362969681409851, 37.25319992234354061, -2.102939460078765421 ) ) ;
#2524 = CARTESIAN_POINT ( 'NONE',  ( 1.027846397803612311, 23.75319992234354416, 3.346150245485499219 ) ) ;
#2525 = CARTESIAN_POINT ( 'NONE',  ( 4.243569643749996345, -22.67008830622574322, -3.823271248141685508 ) ) ;
#2526 = CARTESIAN_POINT ( 'NONE',  ( 2.500000000000001332, 26.74680007765648071, -0.05647727720535888202 ) ) ;
#2527 = EDGE_CURVE ( 'NONE', #17673, #13336, #2193, .T. ) ;
#2528 = CARTESIAN_POINT ( 'NONE',  ( -2.733110507866328476, 24.87819992234354771, -3.862833514489096398 ) ) ;
#2529 = CARTESIAN_POINT ( 'NONE',  ( -2.000000000000005773, -27.29175211571113735, -8.655704456514076384 ) ) ;
#2530 = ORIENTED_EDGE ( 'NONE', *, *, #14666, .F. ) ;
#2531 = CARTESIAN_POINT ( 'NONE',  ( -4.243569643750005227, -21.75595086079126261, -2.517747677556105845 ) ) ;
#2532 = CARTESIAN_POINT ( 'NONE',  ( 3.481649420246369697, 24.12180007765648071, -1.193696214020541824 ) ) ;
#2533 = TOROIDAL_SURFACE ( 'NONE', #15264, 9.000000000000001776, 0.9999999999999991118 ) ;
#2534 = CARTESIAN_POINT ( 'NONE',  ( 2.121784821874994176, -27.56671030237578179, -8.680627135892345692 ) ) ;
#2535 = CARTESIAN_POINT ( 'NONE',  ( 12.00000000000000178, 48.00000000000000000, 15.00000000000000000 ) ) ;
#2536 = DIRECTION ( 'NONE',  ( -4.915049848600951133E-16, 0.000000000000000000, -1.000000000000000000 ) ) ;
#2537 = DIRECTION ( 'NONE',  ( -0.000000000000000000, -1.000000000000000000, -0.000000000000000000 ) ) ;
#2538 = ORIENTED_EDGE ( 'NONE', *, *, #9374, .F. ) ;
#2539 = ORIENTED_EDGE ( 'NONE', *, *, #17953, .T. ) ;
#2540 = CARTESIAN_POINT ( 'NONE',  ( -3.500000000000000444, 17.99680007765647716, 0.05647727720536892260 ) ) ;
#2541 = CARTESIAN_POINT ( 'NONE',  ( 4.898587196589414801E-16, 0.000000000000000000, -4.000000000000000000 ) ) ;
#2542 = EDGE_CURVE ( 'NONE', #9873, #8670, #16620, .T. ) ;
#2543 = CARTESIAN_POINT ( 'NONE',  ( -1.661723472263481630E-14, -21.28506360070608139, -13.09052826979102946 ) ) ;
#2544 = DIRECTION ( 'NONE',  ( -0.000000000000000000, -0.5735764363510414965, -0.8191520442889950182 ) ) ;
#2545 = ORIENTED_EDGE ( 'NONE', *, *, #4076, .F. ) ;
#2546 = CARTESIAN_POINT ( 'NONE',  ( 1.593127413382953383, 35.37819992234354061, -2.091722143975172532 ) ) ;
#2547 = EDGE_CURVE ( 'NONE', #13037, #6995, #5736, .T. ) ;
#2548 = CARTESIAN_POINT ( 'NONE',  ( -2.121784821874996396, -21.41682399769271328, -12.71214960309270303 ) ) ;
#2549 = CARTESIAN_POINT ( 'NONE',  ( 1.135272562821090458, 29.74680007765647716, 3.311245368580554072 ) ) ;
#2550 = ADVANCED_FACE ( 'NONE', ( #12555, #1079 ), #9859, .T. ) ;
#2551 = CARTESIAN_POINT ( 'NONE',  ( 3.518350579753605434, 25.62819992234353705, -1.080741659609877114 ) ) ;
#2552 = DIRECTION ( 'NONE',  ( -0.000000000000000000, 1.000000000000000000, -0.000000000000000000 ) ) ;
#2553 = CARTESIAN_POINT ( 'NONE',  ( 8.499999999999994671, 13.00000000000000000, 22.64999999999999503 ) ) ;
#2554 = CARTESIAN_POINT ( 'NONE',  ( -4.243569643749997233, -22.68915988664961247, -12.39348851099227389 ) ) ;
#2555 = CARTESIAN_POINT ( 'NONE',  ( 0.000000000000000000, -15.45745613286698550, -10.86990606519495195 ) ) ;
#2556 = CARTESIAN_POINT ( 'NONE',  ( -3.607379964056306676, 25.24680007765648071, 2.690724712371306282 ) ) ;
#2557 = CARTESIAN_POINT ( 'NONE',  ( -3.999999999999997335, -18.81978933645070029, -6.622282467816152263 ) ) ;
#2558 = DIRECTION ( 'NONE',  ( 0.000000000000000000, 0.000000000000000000, 1.000000000000000000 ) ) ;
#2559 =( BOUNDED_CURVE ( )  B_SPLINE_CURVE ( 2, ( #5335, #1170, #5146, #2658, #3851, #7923, #803, #12279, #10804 ),
 .UNSPECIFIED., .F., .F. ) 
 B_SPLINE_CURVE_WITH_KNOTS ( ( 3, 2, 2, 2, 3 ),
 ( 0.9396551724137931494, 0.9425287356321838672, 0.9482758620689655249, 0.9540229885057470716, 0.9568965517241379004 ),
 .UNSPECIFIED. ) 
 CURVE ( )  GEOMETRIC_REPRESENTATION_ITEM ( )  RATIONAL_B_SPLINE_CURVE ( ( 0.9330127018922194093, 0.9330127018922206306, 1.000000000000000000, 0.8660254037844387076, 1.000000000000000000, 0.8660254037844387076, 1.000000000000000000, 0.9330127018922194093, 0.9330127018922194093 ) ) 
 REPRESENTATION_ITEM ( '' )  );
#2560 = CARTESIAN_POINT ( 'NONE',  ( -2.121784821874996396, -18.83573003411303048, -9.025965403792225672 ) ) ;
#2561 = CIRCLE ( 'NONE', #12897, 0.9999999999999991118 ) ;
#2562 = CARTESIAN_POINT ( 'NONE',  ( 0.000000000000000000, 9.254131787996968228, 30.52396275209373044 ) ) ;
#2563 = DIRECTION ( 'NONE',  ( 0.000000000000000000, -1.000000000000000000, 0.000000000000000000 ) ) ;
#2564 = CARTESIAN_POINT ( 'NONE',  ( 0.05938372350926800214, 37.37180007765647360, 2.628655560595669183 ) ) ;
#2565 = CIRCLE ( 'NONE', #16784, 8.000000000000001776 ) ;
#2566 = FACE_OUTER_BOUND ( 'NONE', #11461, .T. ) ;
#2567 = CARTESIAN_POINT ( 'NONE',  ( -1.135272562821090014, 35.99680007765648071, -3.311245368580554072 ) ) ;
#2568 = CARTESIAN_POINT ( 'NONE',  ( 0.000000000000000000, -3.999999999999991562, 11.59510085796834566 ) ) ;
#2569 = ITEM_DEFINED_TRANSFORMATION ( 'NONE', 'NONE', #16367,  #16940 ) ;
#2570 = CARTESIAN_POINT ( 'NONE',  ( -1.557381532822000203, 15.00000000000000888, -3.376484385459055826 ) ) ;
#2571 = VERTEX_POINT ( 'NONE', #8377 ) ;
#2572 = CARTESIAN_POINT ( 'NONE',  ( -4.243569643749998122, -19.33373773399602058, -7.601449051901652432 ) ) ;
#2573 = CARTESIAN_POINT ( 'NONE',  ( -2.211161402132902243, 28.37180007765647716, -2.942372952327172886 ) ) ;
#2574 = CYLINDRICAL_SURFACE ( 'NONE', #6163, 4.000000000000000000 ) ;
#2575 = AXIS2_PLACEMENT_3D ( 'NONE', #17037, #5790, #11166 ) ;
#2576 = CARTESIAN_POINT ( 'NONE',  ( -4.243569643750004339, -28.43453149155370241, -12.05574929324608924 ) ) ;
#2577 = CARTESIAN_POINT ( 'NONE',  ( -8.500000000000010658, 14.80000000000000071, 20.49999999999998934 ) ) ;
#2578 = DIRECTION ( 'NONE',  ( -0.000000000000000000, -0.000000000000000000, 1.000000000000000000 ) ) ;
#2579 = DIRECTION ( 'NONE',  ( -1.000000000000000000, -0.000000000000000000, -0.000000000000000000 ) ) ;
#2580 = CARTESIAN_POINT ( 'NONE',  ( -4.243569643750005227, -28.17642209519573271, -11.68713087331604150 ) ) ;
#2581 = EDGE_LOOP ( 'NONE', ( #12518, #916, #2405, #9613 ) ) ;
#2582 = DIRECTION ( 'NONE',  ( -1.000000000000000000, 0.000000000000000000, 4.336808689942021680E-16 ) ) ;
#2583 = CARTESIAN_POINT ( 'NONE',  ( 2.000000000000004441, -19.48709775713304637, -9.588456612235146892 ) ) ;
#2584 = CARTESIAN_POINT ( 'NONE',  ( -2.055738996568313048, 15.74680007765648071, -1.423772053676023441 ) ) ;
#2585 = ORIENTED_EDGE ( 'NONE', *, *, #4609, .T. ) ;
#2586 = CARTESIAN_POINT ( 'NONE',  ( -4.000000000000007105, 6.938893903907228378E-15, 30.00000000000000000 ) ) ;
#2587 = EDGE_CURVE ( 'NONE', #15966, #16586, #14040, .T. ) ;
#2588 = CARTESIAN_POINT ( 'NONE',  ( -1.444289557195956863, 31.50319992234354416, 4.262301884875733471 ) ) ;
#2589 = DIRECTION ( 'NONE',  ( -1.000000000000000000, -0.000000000000000000, -0.000000000000000000 ) ) ;
#2590 = AXIS2_PLACEMENT_3D ( 'NONE', #17954, #2467, #8095 ) ;
#2591 = CARTESIAN_POINT ( 'NONE',  ( -1.593127413382952939, 26.62819992234354416, 2.091722143975172532 ) ) ;
#2592 = EDGE_CURVE ( 'NONE', #2690, #12581, #2831, .T. ) ;
#2593 = ORIENTED_EDGE ( 'NONE', *, *, #17161, .T. ) ;
#2594 = CARTESIAN_POINT ( 'NONE',  ( -4.243569643750004339, -28.20868576974048025, -11.73320817580729525 ) ) ;
#2595 = CARTESIAN_POINT ( 'NONE',  ( -1.336863392178478716, 27.49680007765647360, 4.297206761780677731 ) ) ;
#2596 = CARTESIAN_POINT ( 'NONE',  ( 2.000000000000004441, -18.39013282190673237, -8.021828326525680453 ) ) ;
#2597 = ORIENTED_EDGE ( 'NONE', *, *, #842, .T. ) ;
#2598 = CARTESIAN_POINT ( 'NONE',  ( -11.99999999999999822, 48.00000000000000000, 15.00000000000000000 ) ) ;
#2599 = CARTESIAN_POINT ( 'NONE',  ( -4.000000000000004441, -25.91569448259783215, -8.703649444160298287 ) ) ;
#2600 = CYLINDRICAL_SURFACE ( 'NONE', #15004, 4.000000000000000000 ) ;
#2601 = DIRECTION ( 'NONE',  ( 1.000000000000000000, 0.000000000000000000, 0.000000000000000000 ) ) ;
#2602 = CARTESIAN_POINT ( 'NONE',  ( 2.121784821875004390, -19.42723073410004986, -9.870715949465248329 ) ) ;
#2603 = ORIENTED_EDGE ( 'NONE', *, *, #802, .T. ) ;
#2604 = CARTESIAN_POINT ( 'NONE',  ( -1.661723472263481630E-14, -20.05904396871067874, -11.33959077613006450 ) ) ;
#2605 = ORIENTED_EDGE ( 'NONE', *, *, #17223, .T. ) ;
#2606 = CARTESIAN_POINT ( 'NONE',  ( 3.999999999999996447, -26.34587680986112090, -9.318013477377038001 ) ) ;
#2607 = DIRECTION ( 'NONE',  ( -0.000000000000000000, -0.5735764363510414965, -0.8191520442889950182 ) ) ;
#2608 = DIRECTION ( 'NONE',  ( -1.000000000000000000, 8.673617379884035472E-16, 0.000000000000000000 ) ) ;
#2609 = CARTESIAN_POINT ( 'NONE',  ( 0.000000000000000000, -1.759474945355381292, 3.047500000000002540 ) ) ;
#2610 = ORIENTED_EDGE ( 'NONE', *, *, #3037, .T. ) ;
#2611 = CARTESIAN_POINT ( 'NONE',  ( 2.864755990943222308, 38.00319992234354061, -2.011557305968548093 ) ) ;
#2612 = CARTESIAN_POINT ( 'NONE',  ( 2.115076519116425580, 18.62819992234354771, 3.012182706137062294 ) ) ;
#2613 = EDGE_CURVE ( 'NONE', #7280, #11197, #10033, .T. ) ;
#2614 = CARTESIAN_POINT ( 'NONE',  ( 4.730628863548789710E-15, -16.30511083791103744, -7.547611698733671659 ) ) ;
#2615 = CARTESIAN_POINT ( 'NONE',  ( 1.497042530366477164, 33.87180007765647360, -2.161531897785062384 ) ) ;
#2616 = CARTESIAN_POINT ( 'NONE',  ( 3.607379964056363075, 26.00319992234354771, 2.690724712371229010 ) ) ;
#2617 = VECTOR ( 'NONE', #12733, 1000.000000000000000 ) ;
#2618 = CARTESIAN_POINT ( 'NONE',  ( -5.279047395330986450E-15, -28.99044649497685455, -9.068532494787179488 ) ) ;
#2619 = EDGE_LOOP ( 'NONE', ( #9085, #6999 ) ) ;
#2620 = CARTESIAN_POINT ( 'NONE',  ( -2.000000000000005773, -28.38871705093744779, -10.22233274222354460 ) ) ;
#2621 = CARTESIAN_POINT ( 'NONE',  ( -1.135272562821090014, 18.49680007765648071, -3.311245368580554072 ) ) ;
#2622 = FACE_OUTER_BOUND ( 'NONE', #8437, .T. ) ;
#2623 = CARTESIAN_POINT ( 'NONE',  ( 2.121784821875004390, -19.39496705955529876, -9.824638646973991030 ) ) ;
#2624 = DIRECTION ( 'NONE',  ( 0.000000000000000000, 0.000000000000000000, 1.000000000000000000 ) ) ;
#2625 = DIRECTION ( 'NONE',  ( -1.000000000000000000, 0.000000000000000000, -0.000000000000000000 ) ) ;
#2626 = CARTESIAN_POINT ( 'NONE',  ( 8.500000000000019540, 10.00000000000000000, 18.49999999999998934 ) ) ;
#2627 = CIRCLE ( 'NONE', #12965, 10.00000000000000178 ) ;
#2628 = ORIENTED_EDGE ( 'NONE', *, *, #12876, .F. ) ;
#2629 = AXIS2_PLACEMENT_3D ( 'NONE', #10208, #14504, #12903 ) ;
#2630 = ORIENTED_EDGE ( 'NONE', *, *, #4559, .F. ) ;
#2631 = CARTESIAN_POINT ( 'NONE',  ( 4.898587196589414801E-16, 5.000000000000000000, 4.000000000000001776 ) ) ;
#2632 = DIRECTION ( 'NONE',  ( -1.000000000000000000, 0.000000000000000000, 0.000000000000000000 ) ) ;
#2633 = DIRECTION ( 'NONE',  ( -0.000000000000000000, -1.000000000000000000, -0.000000000000000000 ) ) ;
#2634 = ORIENTED_EDGE ( 'NONE', *, *, #5808, .F. ) ;
#2635 = CARTESIAN_POINT ( 'NONE',  ( 2.500000000000001332, 35.75319992234354061, 0.05647727720530566764 ) ) ;
#2636 = CARTESIAN_POINT ( 'NONE',  ( -2.121784821875005722, -27.09350974238616416, -8.004826699353927211 ) ) ;
#2637 = CARTESIAN_POINT ( 'NONE',  ( 2.211161402132902243, 34.62180007765648071, 2.942372952327172442 ) ) ;
#2638 = CARTESIAN_POINT ( 'NONE',  ( -2.115076519116425580, 29.87819992234353350, -3.012182706137062738 ) ) ;
#2639 = CARTESIAN_POINT ( 'NONE',  ( -5.577813053751546416E-15, -25.64435008597530796, -5.368660209577289955 ) ) ;
#2640 = DIRECTION ( 'NONE',  ( 0.000000000000000000, 0.000000000000000000, -1.000000000000000000 ) ) ;
#2641 = AXIS2_PLACEMENT_3D ( 'NONE', #13467, #2087, #11888 ) ;
#2642 = CARTESIAN_POINT ( 'NONE',  ( -5.330712181944245322E-15, -27.59151744226915781, -6.580310347463352194 ) ) ;
#2643 = AXIS2_PLACEMENT_3D ( 'NONE', #5642, #9539, #8055 ) ;
#2644 = EDGE_CURVE ( 'NONE', #10757, #6383, #10125, .T. ) ;
#2645 = EDGE_CURVE ( 'NONE', #5462, #11668, #14512, .T. ) ;
#2646 = CARTESIAN_POINT ( 'NONE',  ( 0.000000000000000000, 9.254131787996968228, 30.52396275209373044 ) ) ;
#2647 = EDGE_CURVE ( 'NONE', #11633, #14859, #17210, .T. ) ;
#2648 = CARTESIAN_POINT ( 'NONE',  ( 9.000000000000003553, -4.000000000000000000, 30.00000000000000000 ) ) ;
#2649 = VECTOR ( 'NONE', #13207, 999.9999999999998863 ) ;
#2650 = CARTESIAN_POINT ( 'NONE',  ( -4.243569643750000786, -22.06123700099670870, -7.225231581817909365 ) ) ;
#2651 = CARTESIAN_POINT ( 'NONE',  ( -9.184850993605147944E-16, 46.00000000000000000, -2.500000000000000000 ) ) ;
#2652 = EDGE_CURVE ( 'NONE', #13721, #9512, #7748, .T. ) ;
#2653 = CIRCLE ( 'NONE', #13589, 0.9999999999999991118 ) ;
#2654 = CARTESIAN_POINT ( 'NONE',  ( -1.497042530366522461, 14.87819992234354594, -2.161531897785030409 ) ) ;
#2655 = AXIS2_PLACEMENT_3D ( 'NONE', #4723, #837, #2056 ) ;
#2656 = CARTESIAN_POINT ( 'NONE',  ( 1.999999999999994449, -26.28082364734737908, -7.211948979461484832 ) ) ;
#2657 = CARTESIAN_POINT ( 'NONE',  ( 1.135272562821090458, 39.74680007765648071, 3.311245368580554072 ) ) ;
#2658 = CARTESIAN_POINT ( 'NONE',  ( -3.999999999999997335, -18.23904319394032569, -5.792891021966779519 ) ) ;
#2659 = CONTEXT_DEPENDENT_SHAPE_REPRESENTATION ( #10790, #2339 ) ;
#2660 = CARTESIAN_POINT ( 'NONE',  ( -1.139492713648220912, 15.00000000000000533, -3.396762047727180267 ) ) ;
#2661 = EDGE_CURVE ( 'NONE', #4032, #9180, #11593, .T. ) ;
#2662 = VERTEX_POINT ( 'NONE', #3290 ) ;
#2663 = CARTESIAN_POINT ( 'NONE',  ( 4.243569643750003451, -19.67788359580665869, -8.092940278475046156 ) ) ;
#2664 = CARTESIAN_POINT ( 'NONE',  ( -3.518350579753630747, 23.12180007765647716, -1.080741659609802729 ) ) ;
#2665 = AXIS2_PLACEMENT_3D ( 'NONE', #15563, #11280, #2515 ) ;
#2666 = DIRECTION ( 'NONE',  ( -0.000000000000000000, 1.000000000000000000, -0.000000000000000000 ) ) ;
#2667 = MECHANICAL_DESIGN_GEOMETRIC_PRESENTATION_REPRESENTATION (  '', ( #6507 ), #16887 ) ;
#2668 = CARTESIAN_POINT ( 'NONE',  ( -5.330712181944246111E-15, -30.39845712766207697, -10.58903566420262088 ) ) ;
#2669 = DIRECTION ( 'NONE',  ( 0.000000000000000000, 0.000000000000000000, 1.000000000000000000 ) ) ;
#2670 = CARTESIAN_POINT ( 'NONE',  ( 8.000000000000001776, 36.39999999999999147, -2.500000000000002220 ) ) ;
#2671 = CARTESIAN_POINT ( 'NONE',  ( 8.499999999999994671, 14.99364916731036956, 22.64999999999999147 ) ) ;
#2672 = CARTESIAN_POINT ( 'NONE',  ( 4.730628863548789710E-15, -22.49973635050228538, -16.39445377705482088 ) ) ;
#2673 = EDGE_LOOP ( 'NONE', ( #3283, #7736, #15748, #15408, #4894, #14015, #8873, #17450, #432, #16336, #463, #11979, #6964, #11277, #4568, #2179, #2848, #5279, #12708, #1226, #2593, #9073, #15890, #4055, #12737, #421, #6870, #8259, #3891, #1864, #2605, #9159, #18245, #5070, #8599, #15145, #15010, #17984, #6949, #12616, #15685, #7296, #18358, #10543, #12560, #3536, #15425, #2017, #12591, #536, #18329, #15390, #5361, #4209, #17207, #5938, #2813, #15488, #8213, #312, #15772, #5990, #11315, #6824 ) ) ;
#2674 = CARTESIAN_POINT ( 'NONE',  ( 0.000000000000000000, 33.00000000000000000, 0.000000000000000000 ) ) ;
#2675 = CARTESIAN_POINT ( 'NONE',  ( 4.713407268011036227E-15, -17.74538514514100740, -9.114192170640368573 ) ) ;
#2676 = CARTESIAN_POINT ( 'NONE',  ( 3.481649420246369697, 36.62180007765648071, -1.193696214020541824 ) ) ;
#2677 = ORIENTED_EDGE ( 'NONE', *, *, #5186, .T. ) ;
#2678 = CARTESIAN_POINT ( 'NONE',  ( 1.071796769724495224, -19.03813308399763571, -9.881578931065789106 ) ) ;
#2679 = SHAPE_REPRESENTATION_RELATIONSHIP ( 'NONE' , 'NONE' ,  #10877, #16698 ) ;
#2680 = AXIS2_PLACEMENT_3D ( 'NONE', #17603, #6529, #12085 ) ;
#2681 = CARTESIAN_POINT ( 'NONE',  ( 3.673772985318219053, 16.99680007765647716, 2.599342558260951730 ) ) ;
#2682 = UNCERTAINTY_MEASURE_WITH_UNIT (LENGTH_MEASURE( 1.000000000000000082E-05 ), #8615, 'distance_accuracy_value', 'NONE');
#2683 = CARTESIAN_POINT ( 'NONE',  ( -8.500000000000005329, 10.00000000000000000, -20.49999999999999645 ) ) ;
#2684 = CARTESIAN_POINT ( 'NONE',  ( 1.497042530366522461, 33.62819992234354771, 2.161531897785029965 ) ) ;
#2685 = VERTEX_POINT ( 'NONE', #5695 ) ;
#2686 = CARTESIAN_POINT ( 'NONE',  ( 2.121784821875004390, -22.78265288675364175, -14.66275540855586890 ) ) ;
#2687 = CARTESIAN_POINT ( 'NONE',  ( -1.444289557196047014, 28.49680007765648071, -4.262301884875704161 ) ) ;
#2688 = EDGE_CURVE ( 'NONE', #2662, #16507, #13972, .T. ) ;
#2689 = CARTESIAN_POINT ( 'NONE',  ( 4.730628863548789710E-15, -23.04821881776296877, -17.17776791940616832 ) ) ;
#2690 = VERTEX_POINT ( 'NONE', #8733 ) ;
#2691 = PLANE ( 'NONE',  #15696 ) ;
#2692 = CARTESIAN_POINT ( 'NONE',  ( 4.898587196589413815E-16, 2.700915433685006750, 35.11257424290206330 ) ) ;
#2693 = CARTESIAN_POINT ( 'NONE',  ( 4.000000000000000000, -2.639212418033078489, -1.523749999999996829 ) ) ;
#2694 = AXIS2_PLACEMENT_3D ( 'NONE', #12818, #14397, #8543 ) ;
#2695 = DIRECTION ( 'NONE',  ( 0.000000000000000000, 0.000000000000000000, 1.000000000000000000 ) ) ;
#2696 = CARTESIAN_POINT ( 'NONE',  ( 2.121784821874994176, -25.79220820241474854, -6.146375498873266174 ) ) ;
#2697 = ORIENTED_EDGE ( 'NONE', *, *, #11288, .T. ) ;
#2698 = CARTESIAN_POINT ( 'NONE',  ( 0.000000000000000000, 48.00000000000000000, 0.000000000000000000 ) ) ;
#2699 = ORIENTED_EDGE ( 'NONE', *, *, #6147, .F. ) ;
#2700 = CARTESIAN_POINT ( 'NONE',  ( -3.999999999999997335, -22.94953967817820129, -12.52017718669691604 ) ) ;
#2701 = CARTESIAN_POINT ( 'NONE',  ( -5.000000000000001776, 0.000000000000000000, 5.000000000000000888 ) ) ;
#2702 = DIRECTION ( 'NONE',  ( 0.000000000000000000, 0.000000000000000000, 1.000000000000000000 ) ) ;
#2703 = ORIENTED_EDGE ( 'NONE', *, *, #3889, .F. ) ;
#2704 = CARTESIAN_POINT ( 'NONE',  ( -4.481649420246396787, 17.12819992234354416, -1.518615910253363399 ) ) ;
#2705 = CARTESIAN_POINT ( 'NONE',  ( -0.05938372350920064630, 18.87819992234354771, 3.680117784833935701 ) ) ;
#2706 = CARTESIAN_POINT ( 'NONE',  ( 4.713407268011036227E-15, -22.13324488322647454, -15.38070530945117831 ) ) ;
#2707 = CARTESIAN_POINT ( 'NONE',  ( -2.481649420246374138, 30.37180007765648426, 0.8687765177876256573 ) ) ;
#2708 = CIRCLE ( 'NONE', #3582, 1.250000000000000222 ) ;
#2709 = CARTESIAN_POINT ( 'NONE',  ( -3.607379964056363075, 24.75319992234354416, -2.690724712371229899 ) ) ;
#2710 = CARTESIAN_POINT ( 'NONE',  ( 3.999999999999996447, -26.79756825278262511, -9.963095711247856201 ) ) ;
#2711 = ORIENTED_EDGE ( 'NONE', *, *, #4160, .F. ) ;
#2712 = EDGE_CURVE ( 'NONE', #17357, #5462, #13674, .T. ) ;
#2713 = CARTESIAN_POINT ( 'NONE',  ( 4.299564228933482956E-15, -22.38202853593239183, -14.65715655550049590 ) ) ;
#2714 = CARTESIAN_POINT ( 'NONE',  ( 3.500000000000000444, 21.74680007765647716, -0.05647727720536935281 ) ) ;
#2715 = CARTESIAN_POINT ( 'NONE',  ( -4.243569643749998122, -21.10823983395705383, -10.13570068892073195 ) ) ;
#2716 = EDGE_CURVE ( 'NONE', #5029, #13163, #321, .T. ) ;
#2717 = STYLED_ITEM ( 'NONE', ( #12687 ), #5178 ) ;
#2718 = DIRECTION ( 'NONE',  ( 0.000000000000000000, 0.000000000000000000, 1.000000000000000000 ) ) ;
#2719 = ADVANCED_FACE ( 'NONE', ( #4664 ), #12725, .T. ) ;
#2720 = LINE ( 'NONE', #14102, #15780 ) ;
#2721 = CARTESIAN_POINT ( 'NONE',  ( -8.500000000000005329, 15.00000000000000178, -20.49999999999999645 ) ) ;
#2722 = ORIENTED_EDGE ( 'NONE', *, *, #14043, .T. ) ;
#2723 = ORIENTED_EDGE ( 'NONE', *, *, #6265, .T. ) ;
#2724 = CARTESIAN_POINT ( 'NONE',  ( 3.500000000000000444, 24.24680007765647716, -0.05647727720536935281 ) ) ;
#2725 = CARTESIAN_POINT ( 'NONE',  ( 4.299564228933482956E-15, -18.70396963712639504, -9.404344070490550322 ) ) ;
#2726 = DIRECTION ( 'NONE',  ( -1.000000000000000000, 0.000000000000000000, 4.336808689942021680E-16 ) ) ;
#2727 = DIRECTION ( 'NONE',  ( -0.000000000000000000, -1.000000000000000000, -0.000000000000000000 ) ) ;
#2728 = EDGE_LOOP ( 'NONE', ( #10209, #9209, #13408, #619 ) ) ;
#2729 = CARTESIAN_POINT ( 'NONE',  ( 1.497042530366522461, 36.12819992234354771, 2.161531897785029965 ) ) ;
#2730 = CARTESIAN_POINT ( 'NONE',  ( -4.243569643750005227, -24.56289054618417111, -6.526472994295373198 ) ) ;
#2731 = CARTESIAN_POINT ( 'NONE',  ( -3.500000000000000444, 30.49680007765647716, 0.05647727720536892260 ) ) ;
#2732 = CARTESIAN_POINT ( 'NONE',  ( -2.864755990943222308, 29.25319992234354416, 2.011557305968548093 ) ) ;
#2733 = CARTESIAN_POINT ( 'NONE',  ( -5.577813053751546416E-15, -25.45076803941176991, -5.092196395636519490 ) ) ;
#2734 = CARTESIAN_POINT ( 'NONE',  ( -4.000000000000003553, 6.938893903907228378E-15, 0.000000000000000000 ) ) ;
#2735 = CARTESIAN_POINT ( 'NONE',  ( -4.243569643750005227, -25.36948240980282421, -7.678405556576772817 ) ) ;
#2736 = DIRECTION ( 'NONE',  ( -0.000000000000000000, -0.5735764363510414965, -0.8191520442889950182 ) ) ;
#2737 = AXIS2_PLACEMENT_3D ( 'NONE', #11659, #7020, #14460 ) ;
#2738 = LINE ( 'NONE', #2469, #17193 ) ;
#2739 = CARTESIAN_POINT ( 'NONE',  ( -8.500000000000005329, 0.000000000000000000, -20.49999999999999645 ) ) ;
#2740 = CARTESIAN_POINT ( 'NONE',  ( 4.730628863548789710E-15, -18.11187661241681823, -10.12794063824400581 ) ) ;
#2741 = DIRECTION ( 'NONE',  ( -0.000000000000000000, -0.5735764363510414965, -0.8191520442889950182 ) ) ;
#2742 = AXIS2_PLACEMENT_3D ( 'NONE', #5892, #8758, #11636 ) ;
#2743 = CARTESIAN_POINT ( 'NONE',  ( -0.05938372350921170689, 16.37819992234354416, 2.628655560595669183 ) ) ;
#2744 = CARTESIAN_POINT ( 'NONE',  ( 1.071796769724495224, -17.16683995969741616, -7.209095385566181236 ) ) ;
#2745 = DIRECTION ( 'NONE',  ( 0.000000000000000000, 1.000000000000000000, 0.000000000000000000 ) ) ;
#2746 = CARTESIAN_POINT ( 'NONE',  ( 1.999999999999994449, -28.60380821456909572, -10.52951475883191357 ) ) ;
#2747 = EDGE_CURVE ( 'NONE', #9609, #13697, #8343, .T. ) ;
#2748 = CARTESIAN_POINT ( 'NONE',  ( -8.999999999999996447, -10.00000000000000000, -3.713574246709372417 ) ) ;
#2749 = ADVANCED_FACE ( 'NONE', ( #513 ), #10094, .F. ) ;
#2750 = ORIENTED_EDGE ( 'NONE', *, *, #1841, .F. ) ;
#2751 = TOROIDAL_SURFACE ( 'NONE', #9549, 9.000000000000003553, 0.9999999999999991118 ) ;
#2752 = CARTESIAN_POINT ( 'NONE',  ( -4.243569643749998122, -19.59184713035399383, -7.970067471831701056 ) ) ;
#2753 = CARTESIAN_POINT ( 'NONE',  ( 0.05938372350927906274, 29.87180007765648071, 3.680117784833935701 ) ) ;
#2754 = AXIS2_PLACEMENT_3D ( 'NONE', #7395, #14655, #13054 ) ;
#2755 = CARTESIAN_POINT ( 'NONE',  ( 8.673617379884035472E-15, 10.00000000000000000, -6.999999999999996447 ) ) ;
#2756 = CARTESIAN_POINT ( 'NONE',  ( -1.734723475976807094E-15, 36.39999999999999147, -12.50000000000000000 ) ) ;
#2757 = CARTESIAN_POINT ( 'NONE',  ( 0.000000000000000000, 0.000000000000000000, 6.099999999999999645 ) ) ;
#2758 = DIRECTION ( 'NONE',  ( -1.000000000000000000, 0.000000000000000000, 4.336808689942021680E-16 ) ) ;
#2759 = CARTESIAN_POINT ( 'NONE',  ( 1.071796769724485232, -29.31088228406247609, -10.60501085993131909 ) ) ;
#2760 = CARTESIAN_POINT ( 'NONE',  ( -2.121784821875005722, -29.41649430960788081, -11.32239247872435506 ) ) ;
#2761 = ORIENTED_EDGE ( 'NONE', *, *, #5135, .T. ) ;
#2762 = CARTESIAN_POINT ( 'NONE',  ( 4.299564228933482956E-15, -17.73605940148895854, -8.022024996759636650 ) ) ;
#2763 = AXIS2_PLACEMENT_3D ( 'NONE', #16571, #14992, #8293 ) ;
#2764 = CARTESIAN_POINT ( 'NONE',  ( 3.999999999999996447, -23.24856405356549871, -4.894592438216464281 ) ) ;
#2765=STYLED_ITEM('',(#18396),#2247);
#2766 = CARTESIAN_POINT ( 'NONE',  ( 0.8262555684461332373, 17.24680007765648071, 2.360188852285403982 ) ) ;
#2767 = ORIENTED_EDGE ( 'NONE', *, *, #14672, .F. ) ;
#2768 = CARTESIAN_POINT ( 'NONE',  ( -1.071796769724496334, -25.46229474013060567, -5.108658230292436819 ) ) ;
#2769 = EDGE_CURVE ( 'NONE', #2986, #5758, #16423, .T. ) ;
#2770 = EDGE_CURVE ( 'NONE', #8355, #13335, #361, .T. ) ;
#2771 = CARTESIAN_POINT ( 'NONE',  ( -2.829195390882724315, 39.12819992234354771, 3.793023760679264722 ) ) ;
#2772 = CARTESIAN_POINT ( 'NONE',  ( -13.00000000000000178, 15.00000000000000178, -25.00000000000000355 ) ) ;
#2773 = EDGE_CURVE ( 'NONE', #1402, #3198, #12787, .T. ) ;
#2774 = CARTESIAN_POINT ( 'NONE',  ( 0.05938372350921204690, 32.62819992234354771, -2.628655560595669183 ) ) ;
#2775 = ORIENTED_EDGE ( 'NONE', *, *, #17964, .T. ) ;
#2776 = CARTESIAN_POINT ( 'NONE',  ( -5.330712181944246111E-15, -28.88206442405900987, -8.423402447113589986 ) ) ;
#2777 = CARTESIAN_POINT ( 'NONE',  ( 2.733110507866247652, 36.37180007765647360, -3.862833514489153686 ) ) ;
#2778 = ORIENTED_EDGE ( 'NONE', *, *, #9638, .T. ) ;
#2779 = CIRCLE ( 'NONE', #8093, 6.099999999999999645 ) ;
#2780 = CARTESIAN_POINT ( 'NONE',  ( -15.00000000000000178, 13.00000000000000178, 24.99999999999999645 ) ) ;
#2781 = SURFACE_SIDE_STYLE ('',( #11192 ) ) ;
#2782 = DIRECTION ( 'NONE',  ( -3.373073425510457965E-16, 0.000000000000000000, -1.000000000000000000 ) ) ;
#2783 = CARTESIAN_POINT ( 'NONE',  ( -9.184850993605147944E-16, 13.00000000000000178, -10.50000000000000000 ) ) ;
#2784 = CARTESIAN_POINT ( 'NONE',  ( -4.243569643749997233, -20.10806592306992613, -8.707304311691796528 ) ) ;
#2785 = ORIENTED_EDGE ( 'NONE', *, *, #342, .T. ) ;
#2786 = DIRECTION ( 'NONE',  ( 0.000000000000000000, -0.000000000000000000, -1.000000000000000000 ) ) ;
#2787 = ORIENTED_EDGE ( 'NONE', *, *, #11924, .T. ) ;
#2788 = CARTESIAN_POINT ( 'NONE',  ( -4.000000000000000888, -24.30356238220903364, -10.42760410546358152 ) ) ;
#2789 = DIRECTION ( 'NONE',  ( -1.000000000000000000, 0.000000000000000000, 4.336808689942021680E-16 ) ) ;
#2790 = AXIS2_PLACEMENT_3D ( 'NONE', #1248, #15066, #16456 ) ;
#2791 = CARTESIAN_POINT ( 'NONE',  ( 3.673772985318163098, 18.00319992234354416, -2.599342558261029001 ) ) ;
#2792 = CARTESIAN_POINT ( 'NONE',  ( -2.115076519116425580, 17.37819992234354416, -3.012182706137063182 ) ) ;
#2793 = CARTESIAN_POINT ( 'NONE',  ( -4.000000000000000888, -26.62654694943075029, -13.74516988483401114 ) ) ;
#2794 = CARTESIAN_POINT ( 'NONE',  ( 0.05938372350926800214, 37.37180007765647360, 2.628655560595669183 ) ) ;
#2795 = CARTESIAN_POINT ( 'NONE',  ( -4.481649420246396787, 27.12819992234355126, -1.518615910253363399 ) ) ;
#2796 = CARTESIAN_POINT ( 'NONE',  ( -5.279047395330986450E-15, -27.69989951318700250, -7.225440395136942584 ) ) ;
#2797 = ORIENTED_EDGE ( 'NONE', *, *, #16786, .F. ) ;
#2798 = EDGE_CURVE ( 'NONE', #7045, #3783, #12479, .T. ) ;
#2799 = CARTESIAN_POINT ( 'NONE',  ( 1.999999999999994449, -23.69972968376769273, -3.525764780161007472 ) ) ;
#2800 = CARTESIAN_POINT ( 'NONE',  ( 2.115076519116362963, 23.87180007765647005, -3.012182706137107147 ) ) ;
#2801 = DIRECTION ( 'NONE',  ( 0.000000000000000000, 0.000000000000000000, -1.000000000000000000 ) ) ;
#2802 = CARTESIAN_POINT ( 'NONE',  ( -2.121784821875005722, -26.06107215695429247, -6.530353019633736267 ) ) ;
#2803 = FACE_OUTER_BOUND ( 'NONE', #1086, .T. ) ;
#2804 = CYLINDRICAL_SURFACE ( 'NONE', #6304, 4.000000000000000000 ) ;
#2805 = CARTESIAN_POINT ( 'NONE',  ( -1.734723475976807094E-15, 23.19999999999999574, -2.500000000000000000 ) ) ;
#2806 = VERTEX_POINT ( 'NONE', #11584 ) ;
#2807 = ORIENTED_EDGE ( 'NONE', *, *, #17859, .F. ) ;
#2808 = CARTESIAN_POINT ( 'NONE',  ( 3.481649420246369697, 26.62180007765648071, -1.193696214020541824 ) ) ;
#2809 = DIRECTION ( 'NONE',  ( 0.000000000000000000, 0.000000000000000000, -1.000000000000000000 ) ) ;
#2810 = CARTESIAN_POINT ( 'NONE',  ( -13.00000000000000178, 15.00000000000000178, 25.00000000000000355 ) ) ;
#2811 = DIRECTION ( 'NONE',  ( 0.000000000000000000, 0.000000000000000000, -1.000000000000000000 ) ) ;
#2812 = DIRECTION ( 'NONE',  ( 0.000000000000000000, 0.000000000000000000, 1.000000000000000000 ) ) ;
#2813 = ORIENTED_EDGE ( 'NONE', *, *, #16182, .T. ) ;
#2814 = CARTESIAN_POINT ( 'NONE',  ( 3.500000000000000444, 20.75319992234354416, 0.05647727720529520379 ) ) ;
#2815 = CARTESIAN_POINT ( 'NONE',  ( -5.330712181944245322E-15, -27.30114437136644767, -6.165614625042047159 ) ) ;
#2816 = CARTESIAN_POINT ( 'NONE',  ( -2.115076519116362519, 37.62180007765648071, 3.012182706137107147 ) ) ;
#2817 = EDGE_CURVE ( 'NONE', #2141, #14057, #5137, .T. ) ;
#2818 = CARTESIAN_POINT ( 'NONE',  ( 3.481649420246394122, 28.37819992234354416, 1.193696214020467439 ) ) ;
#2819 = CARTESIAN_POINT ( 'NONE',  ( 0.000000000000000000, 16.59999999999999787, 2.500000000000000000 ) ) ;
#2820 = ADVANCED_FACE ( 'NONE', ( #11490 ), #1784, .T. ) ;
#2821 = CARTESIAN_POINT ( 'NONE',  ( 4.243569643750000786, -24.54553994094216307, -10.77318387364461572 ) ) ;
#2822 =( BOUNDED_CURVE ( )  B_SPLINE_CURVE ( 2, ( #18126, #7986, #1139, #1049, #12434, #5302, #6602, #12339, #10953 ),
 .UNSPECIFIED., .F., .F. ) 
 B_SPLINE_CURVE_WITH_KNOTS ( ( 3, 2, 2, 2, 3 ),
 ( 0.7500000000000000000, 0.7528735632183908288, 0.7586206896551723755, 0.7643678160919540332, 0.7672413793103448620 ),
 .UNSPECIFIED. ) 
 CURVE ( )  GEOMETRIC_REPRESENTATION_ITEM ( )  RATIONAL_B_SPLINE_CURVE ( ( 0.9330127018922194093, 0.9330127018922194093, 1.000000000000000000, 0.8660254037844387076, 1.000000000000000000, 0.8660254037844387076, 1.000000000000000000, 0.9330127018922180770, 0.9330127018922194093 ) ) 
 REPRESENTATION_ITEM ( '' )  );
#2823 = CARTESIAN_POINT ( 'NONE',  ( -14.99999999999999645, -4.000000000000000000, 30.00000000000000000 ) ) ;
#2824 = CARTESIAN_POINT ( 'NONE',  ( 4.299564228933482956E-15, -22.38202853593239183, -14.65715655550049590 ) ) ;
#2825 = DIRECTION ( 'NONE',  ( 0.000000000000000000, 0.000000000000000000, -1.000000000000000000 ) ) ;
#2826 = CARTESIAN_POINT ( 'NONE',  ( -2.121784821875005722, -22.96375940065866672, -2.106931980473163879 ) ) ;
#2827 = CARTESIAN_POINT ( 'NONE',  ( 4.000000000000003553, -22.77746674727289289, -12.27443157341021163 ) ) ;
#2828 = EDGE_LOOP ( 'NONE', ( #9130, #7916, #14488, #9475 ) ) ;
#2829 = CARTESIAN_POINT ( 'NONE',  ( -0.8262555684460826111, 19.00319992234354771, 2.360188852285421302 ) ) ;
#2830 = CARTESIAN_POINT ( 'NONE',  ( 4.243569643750000786, -26.32004204090319632, -13.30743551066369257 ) ) ;
#2831 = LINE ( 'NONE', #4482, #15473 ) ;
#2832 = CONTEXT_DEPENDENT_SHAPE_REPRESENTATION ( #2864, #1177 ) ;
#2833 = CARTESIAN_POINT ( 'NONE',  ( -9.178305741915819382, -9.999999999999996447, -2.937604372561400279 ) ) ;
#2834 = EDGE_CURVE ( 'NONE', #7772, #3408, #17185, .T. ) ;
#2835 = VERTEX_POINT ( 'NONE', #4360 ) ;
#2836 = CARTESIAN_POINT ( 'NONE',  ( -4.243569643750000786, -19.77051610831973605, -3.953743104938735708 ) ) ;
#2837 = CARTESIAN_POINT ( 'NONE',  ( -2.798362969681365886, 30.24680007765648071, 2.102939460078824929 ) ) ;
#2838 =( NAMED_UNIT ( * ) PLANE_ANGLE_UNIT ( ) SI_UNIT ( $, .RADIAN. ) );
#2839 = CARTESIAN_POINT ( 'NONE',  ( -2.121784821875005722, -28.64216612053397526, -10.21653721893421363 ) ) ;
#2840 = LINE ( 'NONE', #13873, #2285 ) ;
#2841 = DIRECTION ( 'NONE',  ( -0.000000000000000000, 1.000000000000000000, -0.000000000000000000 ) ) ;
#2842 = AXIS2_PLACEMENT_3D ( 'NONE', #13415, #730, #8868 ) ;
#2843 = CARTESIAN_POINT ( 'NONE',  ( 4.243569643750003451, -22.22671388484159039, -11.73304717528426977 ) ) ;
#2844 = VERTEX_POINT ( 'NONE', #7317 ) ;
#2845 = DIRECTION ( 'NONE',  ( -1.000000000000000000, 0.000000000000000000, 4.336808689942021680E-16 ) ) ;
#2846 = CARTESIAN_POINT ( 'NONE',  ( 4.000000000000003553, -17.87338821647148990, -5.270681594739305531 ) ) ;
#2847 = CARTESIAN_POINT ( 'NONE',  ( -2.864755990943265829, 38.24680007765647360, -2.011557305968488141 ) ) ;
#2848 = ORIENTED_EDGE ( 'NONE', *, *, #9219, .T. ) ;
#2849 = DIRECTION ( 'NONE',  ( -3.373073425510457965E-16, 0.000000000000000000, -1.000000000000000000 ) ) ;
#2850 = CARTESIAN_POINT ( 'NONE',  ( 3.579096709490575479E-14, -26.67678767140717966, -6.843133889297480899 ) ) ;
#2851 = CARTESIAN_POINT ( 'NONE',  ( -0.7188294034286550893, 35.00319992234354771, -2.395093729190349130 ) ) ;
#2852 = ORIENTED_EDGE ( 'NONE', *, *, #10457, .F. ) ;
#2853 = CARTESIAN_POINT ( 'NONE',  ( -4.243569643749998122, -22.17294109393367663, -11.65625167113217664 ) ) ;
#2854 = CARTESIAN_POINT ( 'NONE',  ( 4.481649420246366589, 36.62180007765647360, -1.518615910253458212 ) ) ;
#2855 = CIRCLE ( 'NONE', #493, 2.149999999999995470 ) ;
#2856 = ORIENTED_EDGE ( 'NONE', *, *, #3659, .T. ) ;
#2857 = CARTESIAN_POINT ( 'NONE',  ( 4.000000000000000000, 3.518949890710770134, -4.119968255444916849E-15 ) ) ;
#2858 = EDGE_CURVE ( 'NONE', #4607, #5051, #12979, .T. ) ;
#2859 = CARTESIAN_POINT ( 'NONE',  ( -3.291771655530798757, -28.93493258167780269, -13.02337503524261386 ) ) ;
#2860 = CARTESIAN_POINT ( 'NONE',  ( 9.000000000000000000, 25.39999999999999503, -2.500000000000001332 ) ) ;
#2861 = ADVANCED_FACE ( 'NONE', ( #294 ), #11631, .T. ) ;
#2862 = CARTESIAN_POINT ( 'NONE',  ( 4.243569643749996345, -24.50911775527627157, -6.449677490143276515 ) ) ;
#2863 = ORIENTED_EDGE ( 'NONE', *, *, #1700, .T. ) ;
#2864 =( REPRESENTATION_RELATIONSHIP ('NONE','NONE', #15868, #5306 ) REPRESENTATION_RELATIONSHIP_WITH_TRANSFORMATION ( #3943 )SHAPE_REPRESENTATION_RELATIONSHIP( ) );
#2865 = ADVANCED_FACE ( 'NONE', ( #5667 ), #17853, .T. ) ;
#2866 = DIRECTION ( 'NONE',  ( -0.000000000000000000, -0.5735764363510414965, -0.8191520442889950182 ) ) ;
#2867 = EDGE_LOOP ( 'NONE', ( #15191, #14674, #14931, #512 ) ) ;
#2868 = AXIS2_PLACEMENT_3D ( 'NONE', #7528, #12901, #1898 ) ;
#2869 = CARTESIAN_POINT ( 'NONE',  ( -4.000000000000000888, -24.04545298585106394, -10.05898568553353378 ) ) ;
#2870 = CARTESIAN_POINT ( 'NONE',  ( 8.673617379884035472E-16, -1.899999999999999689, -3.490243377569955568E-16 ) ) ;
#2871 = DIRECTION ( 'NONE',  ( 0.000000000000000000, 0.000000000000000000, 1.000000000000000000 ) ) ;
#2872 = SHAPE_REPRESENTATION_RELATIONSHIP ( 'NONE' , 'NONE' ,  #8990, #12463 ) ;
#2873 = ADVANCED_FACE ( 'NONE', ( #5761 ), #8803, .T. ) ;
#2874 = CARTESIAN_POINT ( 'NONE',  ( -4.481649420246396787, 22.12819992234354416, -1.518615910253363399 ) ) ;
#2875 = CARTESIAN_POINT ( 'NONE',  ( -2.798362969681409851, 24.75319992234354416, -2.102939460078765421 ) ) ;
#2876 = CARTESIAN_POINT ( 'NONE',  ( 3.999999999999996447, -27.89453318800893555, -11.52972399695732264 ) ) ;
#2877 = CARTESIAN_POINT ( 'NONE',  ( 2.500000000000001332, 15.75319992234354594, 0.05647727720530566764 ) ) ;
#2878 = CARTESIAN_POINT ( 'NONE',  ( 1.336863392178569754, 33.75319992234354771, 4.297206761780648421 ) ) ;
#2879 = CARTESIAN_POINT ( 'NONE',  ( 2.000000000000004441, -20.97122678548641872, -11.70801252582615604 ) ) ;
#2880 = ORIENTED_EDGE ( 'NONE', *, *, #15246, .F. ) ;
#2881 = ADVANCED_FACE ( 'NONE', ( #14485 ), #5631, .F. ) ;
#2882 = DIRECTION ( 'NONE',  ( -0.000000000000000000, -0.5735764363510414965, -0.8191520442889950182 ) ) ;
#2883 = VECTOR ( 'NONE', #8870, 1000.000000000000000 ) ;
#2884 = CARTESIAN_POINT ( 'NONE',  ( -3.481649420246369697, 20.37180007765647716, 1.193696214020542490 ) ) ;
#2885 = CARTESIAN_POINT ( 'NONE',  ( -7.467367394352450560, -10.10642962993511951, 13.07819922209348107 ) ) ;
#2886 = CARTESIAN_POINT ( 'NONE',  ( -2.121784821875005722, -26.57729094967022831, -7.267589859493831739 ) ) ;
#2887 = CARTESIAN_POINT ( 'NONE',  ( -1.336863392178478716, 19.99680007765647716, 4.297206761780677731 ) ) ;
#2888 = CYLINDRICAL_SURFACE ( 'NONE', #15699, 2.000000000000001776 ) ;
#2889 = DIRECTION ( 'NONE',  ( -0.000000000000000000, 1.000000000000000000, -0.000000000000000000 ) ) ;
#2890 = ORIENTED_EDGE ( 'NONE', *, *, #6901, .T. ) ;
#2891 = EDGE_LOOP ( 'NONE', ( #2922, #16866, #14458, #10653, #17939 ) ) ;
#2892 = CARTESIAN_POINT ( 'NONE',  ( -2.211161402132902243, 23.37180007765647716, -2.942372952327172886 ) ) ;
#2893 = CYLINDRICAL_SURFACE ( 'NONE', #12525, 4.000000000000000000 ) ;
#2894 = CARTESIAN_POINT ( 'NONE',  ( -2.000000000000005773, -27.29175211571113735, -8.655704456514076384 ) ) ;
#2895 = CARTESIAN_POINT ( 'NONE',  ( -1.071796769724488341, -23.66104881700340457, -16.48378682049481725 ) ) ;
#2896 = VERTEX_POINT ( 'NONE', #11770 ) ;
#2897 = AXIS2_PLACEMENT_3D ( 'NONE', #7667, #6806, #18151 ) ;
#2898 = CARTESIAN_POINT ( 'NONE',  ( -0.05938372350920063936, 16.37819992234354416, 3.680117784833935701 ) ) ;
#2899 = VECTOR ( 'NONE', #10426, 1000.000000000000227 ) ;
#2900 = CARTESIAN_POINT ( 'NONE',  ( 4.730628863548789710E-15, -18.88620480149072378, -11.23379589803414902 ) ) ;
#2901 = CARTESIAN_POINT ( 'NONE',  ( 1.027846397803542144, 38.74680007765647360, -3.346150245485522312 ) ) ;
#2902 = CARTESIAN_POINT ( 'NONE',  ( -2.798362969681409851, 34.75319992234354771, -2.102939460078765421 ) ) ;
#2903 = CARTESIAN_POINT ( 'NONE',  ( 6.123233995736766282E-16, 33.00000000000000000, -5.000000000000000000 ) ) ;
#2904 = DIRECTION ( 'NONE',  ( -0.000000000000000000, -0.5735764363510414965, -0.8191520442889950182 ) ) ;
#2905 = CARTESIAN_POINT ( 'NONE',  ( -5.330712181944245322E-15, -26.04286106412135027, -4.368599827883064890 ) ) ;
#2906 = CLOSED_SHELL ( 'NONE', ( #734, #2306, #10402, #14951, #12373, #4515, #10108, #15058, #1384, #7566, #10663, #2030, #4792, #17733, #3930, #18078 ) ) ;
#2907 = CIRCLE ( 'NONE', #3213, 10.00000000000000000 ) ;
#2908 = TOROIDAL_SURFACE ( 'NONE', #3216, 9.000000000000001776, 0.9999999999999991118 ) ;
#2909 = CARTESIAN_POINT ( 'NONE',  ( 8.500000000000000000, 15.00000000000000000, -22.69999999999999929 ) ) ;
#2910 = CARTESIAN_POINT ( 'NONE',  ( 0.000000000000000000, 0.000000000000000000, 0.000000000000000000 ) ) ;
#2911 = CARTESIAN_POINT ( 'NONE',  ( -3.999999999999997335, -19.07789873280866999, -6.990900887746200887 ) ) ;
#2912 = CARTESIAN_POINT ( 'NONE',  ( 4.243569643750000786, -21.15785411374382363, -5.935067112062737849 ) ) ;
#2913 = CARTESIAN_POINT ( 'NONE',  ( -2.754179286501430735, 15.00000000000001954, -1.305413474713025490 ) ) ;
#2914 =( NAMED_UNIT ( * ) PLANE_ANGLE_UNIT ( ) SI_UNIT ( $, .RADIAN. ) );
#2915 = VERTEX_POINT ( 'NONE', #2157 ) ;
#2916 = CARTESIAN_POINT ( 'NONE',  ( -1.497042530366522461, 22.37819992234354416, -2.161531897785030409 ) ) ;
#2917 = CARTESIAN_POINT ( 'NONE',  ( -5.330712181944245322E-15, -30.65656652402004312, -10.95765408413266861 ) ) ;
#2918 = CARTESIAN_POINT ( 'NONE',  ( -1.135272562821090014, 18.49680007765648071, -3.311245368580554072 ) ) ;
#2919 = CARTESIAN_POINT ( 'NONE',  ( -9.609630862508756977, -9.971178627260298910, 12.03209595322010905 ) ) ;
#2920 = TOROIDAL_SURFACE ( 'NONE', #4376, 9.000000000000001776, 0.9999999999999991118 ) ;
#2921 = DIRECTION ( 'NONE',  ( -0.000000000000000000, -0.5735764363510414965, -0.8191520442889950182 ) ) ;
#2922 = ORIENTED_EDGE ( 'NONE', *, *, #2463, .F. ) ;
#2923 = DIRECTION ( 'NONE',  ( 1.000000000000000000, 0.000000000000000000, 0.000000000000000000 ) ) ;
#2924 = CARTESIAN_POINT ( 'NONE',  ( 2.211161402132902243, 34.62180007765648071, 2.942372952327172442 ) ) ;
#2925 =( BOUNDED_CURVE ( )  B_SPLINE_CURVE ( 2, ( #11167, #6991, #6729, #14050, #12654, #1185, #12385, #18073, #16674 ),
 .UNSPECIFIED., .F., .F. ) 
 B_SPLINE_CURVE_WITH_KNOTS ( ( 3, 2, 2, 2, 3 ),
 ( 0.09482758620689656082, 0.09770114942528736190, 0.1034482758620689641, 0.1091954022988505801, 0.1120689655172413812 ),
 .UNSPECIFIED. ) 
 CURVE ( )  GEOMETRIC_REPRESENTATION_ITEM ( )  RATIONAL_B_SPLINE_CURVE ( ( 0.9330127018922194093, 0.9330127018922195203, 1.000000000000000000, 0.8660254037844387076, 1.000000000000000000, 0.8660254037844387076, 1.000000000000000000, 0.9330127018922194093, 0.9330127018922194093 ) ) 
 REPRESENTATION_ITEM ( '' )  );
#2926 = DIRECTION ( 'NONE',  ( -0.000000000000000000, -0.5000000000000002220, -0.8660254037844384856 ) ) ;
#2927 = CARTESIAN_POINT ( 'NONE',  ( 4.243569643750003451, -23.25915147027346563, -13.20752085500445894 ) ) ;
#2928 = CARTESIAN_POINT ( 'NONE',  ( 0.000000000000000000, 15.00000000000000355, 0.000000000000000000 ) ) ;
#2929 = AXIS2_PLACEMENT_3D ( 'NONE', #10720, #906, #6548 ) ;
#2930 = CARTESIAN_POINT ( 'NONE',  ( 1.300000000000000044, -0.7216878364870317197, 1.250000000000000000 ) ) ;
#2931 = EDGE_CURVE ( 'NONE', #159, #6301, #8225, .T. ) ;
#2932 = DIRECTION ( 'NONE',  ( 0.000000000000000000, 0.000000000000000000, 1.000000000000000000 ) ) ;
#2933 = CARTESIAN_POINT ( 'NONE',  ( -2.121784821874996396, -21.15871460133474713, -12.34353118316265707 ) ) ;
#2934 = DIRECTION ( 'NONE',  ( 0.000000000000000000, 0.000000000000000000, 1.000000000000000000 ) ) ;
#2935 = CARTESIAN_POINT ( 'NONE',  ( 4.000000000000003553, -18.90582580190336515, -6.745155274459496475 ) ) ;
#2936 = CARTESIAN_POINT ( 'NONE',  ( 1.989345975306426206, 21.49680007765648071, -1.515154207786343799 ) ) ;
#2937 = ORIENTED_EDGE ( 'NONE', *, *, #17114, .F. ) ;
#2938 = CARTESIAN_POINT ( 'NONE',  ( -3.500000000000000444, 20.49680007765647716, 0.05647727720536892260 ) ) ;
#2939 = FACE_OUTER_BOUND ( 'NONE', #4064, .T. ) ;
#2940 = AXIS2_PLACEMENT_3D ( 'NONE', #13871, #6818, #12919 ) ;
#2941 = VECTOR ( 'NONE', #8945, 1000.000000000000114 ) ;
#2942 = CARTESIAN_POINT ( 'NONE',  ( -1.071796769724486786, -19.78940787163386972, -10.95451052154410299 ) ) ;
#2943 = CARTESIAN_POINT ( 'NONE',  ( -0.8262555684460826111, 39.00319992234355482, 2.360188852285421302 ) ) ;
#2944 = ORIENTED_EDGE ( 'NONE', *, *, #664, .F. ) ;
#2945 = CARTESIAN_POINT ( 'NONE',  ( -2.121784821875005722, -27.12577341693091171, -8.050904001845182734 ) ) ;
#2946 = CIRCLE ( 'NONE', #7375, 0.9999999999999991118 ) ;
#2947 = CARTESIAN_POINT ( 'NONE',  ( -3.673772985318219053, 30.74680007765647716, -2.599342558260952174 ) ) ;
#2948 = CIRCLE ( 'NONE', #9739, 0.9999999999999991118 ) ;
#2949 = VERTEX_POINT ( 'NONE', #14676 ) ;
#2950 = CARTESIAN_POINT ( 'NONE',  ( -8.000000000000001776, 16.59999999999999787, 2.499999999999998224 ) ) ;
#2951 = CARTESIAN_POINT ( 'NONE',  ( -1.071796769724486786, -19.27318907891793032, -10.21727368168400751 ) ) ;
#2952 = CARTESIAN_POINT ( 'NONE',  ( 4.000000000000003553, -19.35751724482486225, -7.390237508330316452 ) ) ;
#2953 = DIRECTION ( 'NONE',  ( -1.000000000000000000, -0.000000000000000000, -0.000000000000000000 ) ) ;
#2954 = CARTESIAN_POINT ( 'NONE',  ( -11.99999999999999822, 48.00000000000000000, 15.00000000000000000 ) ) ;
#2955 = CARTESIAN_POINT ( 'NONE',  ( 4.730628863548789710E-15, -16.85359330517172083, -8.330925841085024430 ) ) ;
#2956 = ORIENTED_EDGE ( 'NONE', *, *, #4312, .T. ) ;
#2957 = AXIS2_PLACEMENT_3D ( 'NONE', #8286, #17957, #5417 ) ;
#2958 = CARTESIAN_POINT ( 'NONE',  ( -10.00000000000000000, 25.39999999999999503, 2.499999999999996003 ) ) ;
#2959 = ORIENTED_EDGE ( 'NONE', *, *, #12317, .T. ) ;
#2960 = ORIENTED_EDGE ( 'NONE', *, *, #3438, .T. ) ;
#2961 = CARTESIAN_POINT ( 'NONE',  ( 9.999999999999998224, 36.39999999999999147, -2.500000000000001776 ) ) ;
#2962 = CARTESIAN_POINT ( 'NONE',  ( 2.829195390882724759, 20.37819992234354416, -3.793023760679264278 ) ) ;
#2963 = CARTESIAN_POINT ( 'NONE',  ( 2.864755990943222308, 25.50319992234354771, -2.011557305968548093 ) ) ;
#2964 = CARTESIAN_POINT ( 'NONE',  ( -2.518350579753628526, 35.62180007765647360, -0.7558219633769075463 ) ) ;
#2965 = EDGE_CURVE ( 'NONE', #6584, #9470, #7628, .T. ) ;
#2966 = EDGE_LOOP ( 'NONE', ( #739, #16320, #2603, #3520 ) ) ;
#2967 = EDGE_CURVE ( 'NONE', #13882, #9022, #16517, .T. ) ;
#2968 = CARTESIAN_POINT ( 'NONE',  ( -2.733110507866328476, 29.87819992234354416, -3.862833514489096398 ) ) ;
#2969 = CARTESIAN_POINT ( 'NONE',  ( 4.000000000000003553, -22.19672060476252540, -11.44504012756084066 ) ) ;
#2970 = VERTEX_POINT ( 'NONE', #9452 ) ;
#2971 = VECTOR ( 'NONE', #13182, 1000.000000000000000 ) ;
#2972 = DIRECTION ( 'NONE',  ( -0.000000000000000000, 1.000000000000000000, -0.000000000000000000 ) ) ;
#2973 = PRESENTATION_LAYER_ASSIGNMENT (  '', '', ( #18102 ) ) ;
#2974 = CARTESIAN_POINT ( 'NONE',  ( 3.518350579753631191, 29.37180007765647005, 1.080741659609802285 ) ) ;
#2975 = CARTESIAN_POINT ( 'NONE',  ( -9.000000000000001776, 20.99999999999999289, 2.499999999999995559 ) ) ;
#2976 = CARTESIAN_POINT ( 'NONE',  ( -2.121784821875005722, -25.54485336423835307, -5.793116179773641683 ) ) ;
#2977 = CARTESIAN_POINT ( 'NONE',  ( 4.481649420246366589, 31.62180007765647716, -1.518615910253458212 ) ) ;
#2978 = CARTESIAN_POINT ( 'NONE',  ( 1.999999999999994449, -22.86087414489934488, -2.327754914381585660 ) ) ;
#2979 = ORIENTED_EDGE ( 'NONE', *, *, #7152, .T. ) ;
#2980 = EDGE_LOOP ( 'NONE', ( #16300, #15846, #10901, #18032 ) ) ;
#2981 = CARTESIAN_POINT ( 'NONE',  ( 1.027846397803542144, 21.24680007765647716, -3.346150245485522312 ) ) ;
#2982 = CARTESIAN_POINT ( 'NONE',  ( -8.535862155143941976, -10.00000000000000178, 16.49127580077173150 ) ) ;
#2983 = FILL_AREA_STYLE ('',( #17007 ) ) ;
#2984 = DIRECTION ( 'NONE',  ( 0.000000000000000000, 0.000000000000000000, 1.000000000000000000 ) ) ;
#2985 =( LENGTH_UNIT ( ) NAMED_UNIT ( * ) SI_UNIT ( .MILLI., .METRE. ) );
#2986 = VERTEX_POINT ( 'NONE', #17918 ) ;
#2987 = AXIS2_PLACEMENT_3D ( 'NONE', #15725, #429, #6167 ) ;
#2988 = CARTESIAN_POINT ( 'NONE',  ( -1.135272562821019626, 19.00319992234354771, 3.311245368580577164 ) ) ;
#2989 = CARTESIAN_POINT ( 'NONE',  ( -5.330712181944245322E-15, -27.04303497500847797, -5.796996205112000311 ) ) ;
#2990 = CARTESIAN_POINT ( 'NONE',  ( -3.500000000000000444, 37.99680007765647360, 0.05647727720536892260 ) ) ;
#2991 = EDGE_CURVE ( 'NONE', #4808, #13964, #11297, .T. ) ;
#2992 = CARTESIAN_POINT ( 'NONE',  ( 2.798362969681409851, 38.50319992234354061, 2.102939460078764977 ) ) ;
#2993 = DIRECTION ( 'NONE',  ( -0.000000000000000000, 0.000000000000000000, -1.000000000000000000 ) ) ;
#2994 = ADVANCED_FACE ( 'NONE', ( #5189 ), #8149, .T. ) ;
#2995 = CARTESIAN_POINT ( 'NONE',  ( -1.661723472263481630E-14, -21.60770034685848984, -13.55130129571035447 ) ) ;
#2996 = CARTESIAN_POINT ( 'NONE',  ( -2.121784821875005722, -26.09333583149904001, -6.576430322124992678 ) ) ;
#2997 = AXIS2_PLACEMENT_3D ( 'NONE', #3088, #1797, #13190 ) ;
#2998 = DIRECTION ( 'NONE',  ( -0.000000000000000000, 1.000000000000000000, -0.000000000000000000 ) ) ;
#2999 = CARTESIAN_POINT ( 'NONE',  ( -9.000000000000003553, 31.99999999999999289, -2.500000000000001776 ) ) ;
#3000 = LINE ( 'NONE', #7432, #14471 ) ;
#3001 = CARTESIAN_POINT ( 'NONE',  ( -4.243569643750000786, -20.25447122649092790, -4.644902642307576102 ) ) ;
#3002 = LINE ( 'NONE', #7159, #17485 ) ;
#3003 = FILL_AREA_STYLE_COLOUR ( '', #1423 ) ;
#3004 = ORIENTED_EDGE ( 'NONE', *, *, #8865, .F. ) ;
#3005 = CARTESIAN_POINT ( 'NONE',  ( -2.055738996568281518, 19.25319992234354416, 1.423772053676066962 ) ) ;
#3006 = CARTESIAN_POINT ( 'NONE',  ( -2.121784821874996396, -23.99791796127240318, -16.39833380239318217 ) ) ;
#3007 = CARTESIAN_POINT ( 'NONE',  ( 1.135272562821090458, 17.24680007765647716, 3.311245368580554072 ) ) ;
#3008 = PRESENTATION_LAYER_ASSIGNMENT (  '', '', ( #12185 ) ) ;
#3009 = PRODUCT_DEFINITION ( 'UNKNOWN', '', #13086, #5188 ) ;
#3010 = DIRECTION ( 'NONE',  ( -0.000000000000000000, -1.000000000000000000, -0.000000000000000000 ) ) ;
#3011 = FACE_OUTER_BOUND ( 'NONE', #7766, .T. ) ;
#3012 = CIRCLE ( 'NONE', #17864, 2.149999999999995470 ) ;
#3013 = ORIENTED_EDGE ( 'NONE', *, *, #7679, .T. ) ;
#3014 = CARTESIAN_POINT ( 'NONE',  ( 4.243569643750003451, -17.87111782130087434, -5.512611338964712893 ) ) ;
#3015 = CARTESIAN_POINT ( 'NONE',  ( 1.027846397803542144, 36.24680007765648071, -3.346150245485522312 ) ) ;
#3016 = CARTESIAN_POINT ( 'NONE',  ( 2.121784821875004390, -24.07319986854348670, -16.50584750820610580 ) ) ;
#3017 = AXIS2_PLACEMENT_3D ( 'NONE', #11025, #2607, #10937 ) ;
#3018 = CARTESIAN_POINT ( 'NONE',  ( -9.000000000000001776, 36.39999999999999147, 2.499999999999995559 ) ) ;
#3019 = CARTESIAN_POINT ( 'NONE',  ( -4.243569643750000786, -26.19098734272420614, -13.12312630069867225 ) ) ;
#3020 = CARTESIAN_POINT ( 'NONE',  ( -1.734723475976807094E-15, 38.59999999999999432, -2.500000000000000000 ) ) ;
#3021 = CARTESIAN_POINT ( 'NONE',  ( -10.00000000000000000, 40.79999999999999716, 2.499999999999996003 ) ) ;
#3022 = DIRECTION ( 'NONE',  ( -0.000000000000000000, -1.000000000000000000, -0.000000000000000000 ) ) ;
#3023 = CARTESIAN_POINT ( 'NONE',  ( -2.121784821874996396, -21.93304279040865623, -13.44938644295279850 ) ) ;
#3024 = DIRECTION ( 'NONE',  ( 0.000000000000000000, -0.9936001553129347741, -0.1129545544106647093 ) ) ;
#3025 = CARTESIAN_POINT ( 'NONE',  ( 1.999999999999994449, -22.92540149469378363, -2.419909520370864264 ) ) ;
#3026 = CARTESIAN_POINT ( 'NONE',  ( -0.7188294034286043521, 19.99680007765648071, 2.395093729190366005 ) ) ;
#3027 = VERTEX_POINT ( 'NONE', #8057 ) ;
#3028 = CARTESIAN_POINT ( 'NONE',  ( -3.500000000000000444, 25.49680007765647716, 0.05647727720536892260 ) ) ;
#3029 = CARTESIAN_POINT ( 'NONE',  ( -3.999999999999997335, -21.91710209274632604, -11.04570350697672509 ) ) ;
#3030 = AXIS2_PLACEMENT_3D ( 'NONE', #7456, #1481, #7394 ) ;
#3031 = EDGE_CURVE ( 'NONE', #8354, #6383, #8246, .T. ) ;
#3032 = CARTESIAN_POINT ( 'NONE',  ( 8.500000000000001776, 17.19999999999999929, -20.49999999999999645 ) ) ;
#3033 = TOROIDAL_SURFACE ( 'NONE', #12497, 2.200000000000000178, 0.2000000000000000111 ) ;
#3034 = DIRECTION ( 'NONE',  ( 1.000000000000000000, 0.000000000000000000, 0.000000000000000000 ) ) ;
#3035 = CARTESIAN_POINT ( 'NONE',  ( -1.497042530366522461, 37.37819992234354771, -2.161531897785030409 ) ) ;
#3036 =( BOUNDED_CURVE ( )  B_SPLINE_CURVE ( 3, ( #18271, #18365, #161, #12767 ),
 .UNSPECIFIED., .F., .F. ) 
 B_SPLINE_CURVE_WITH_KNOTS ( ( 4, 4 ),
 ( 8.673617379884033500E-16, 1.570796326794896558 ),
 .UNSPECIFIED. ) 
 CURVE ( )  GEOMETRIC_REPRESENTATION_ITEM ( )  RATIONAL_B_SPLINE_CURVE ( ( 1.000000000000000000, 0.8047378541243652705, 0.8047378541243652705, 1.000000000000000000 ) ) 
 REPRESENTATION_ITEM ( '' )  );
#3037 = EDGE_CURVE ( 'NONE', #2269, #2431, #8332, .T. ) ;
#3038 = ORIENTED_EDGE ( 'NONE', *, *, #16535, .T. ) ;
#3039 = CARTESIAN_POINT ( 'NONE',  ( 4.243569643749997233, -26.31588352978205592, -9.030006429653608890 ) ) ;
#3040 = CARTESIAN_POINT ( 'NONE',  ( 0.05938372350929014415, 34.87180007765647360, 4.731580009072201776 ) ) ;
#3041 = EDGE_CURVE ( 'NONE', #9856, #16492, #12322, .T. ) ;
#3042 = ORIENTED_EDGE ( 'NONE', *, *, #1277, .T. ) ;
#3043 = ADVANCED_FACE ( 'NONE', ( #5281 ), #5464, .F. ) ;
#3044 = DIRECTION ( 'NONE',  ( 0.000000000000000000, 0.000000000000000000, 1.000000000000000000 ) ) ;
#3045 = DIRECTION ( 'NONE',  ( -1.000000000000000000, 0.000000000000000000, 4.336808689942021680E-16 ) ) ;
#3046 = AXIS2_PLACEMENT_3D ( 'NONE', #6032, #14041, #11684 ) ;
#3047 = CARTESIAN_POINT ( 'NONE',  ( 6.428571428571431490, -11.73421655796352425, 14.25837509840157935 ) ) ;
#3048 = CIRCLE ( 'NONE', #11605, 8.000000000000000000 ) ;
#3049 = CARTESIAN_POINT ( 'NONE',  ( 4.243569643750000786, -20.93200839193060148, -5.612525994623947412 ) ) ;
#3050 = EDGE_LOOP ( 'NONE', ( #10682, #11607, #3607, #835 ) ) ;
#3051 = DIRECTION ( 'NONE',  ( -3.469446951953613696E-16, -0.000000000000000000, -1.000000000000000000 ) ) ;
#3052 = ORIENTED_EDGE ( 'NONE', *, *, #3999, .F. ) ;
#3053 = VERTEX_POINT ( 'NONE', #15125 ) ;
#3054 = CARTESIAN_POINT ( 'NONE',  ( -8.000000000000000000, 43.00000000000000000, 2.500000000000000000 ) ) ;
#3055 = FILL_AREA_STYLE_COLOUR ( '', #3608 ) ;
#3056 = CARTESIAN_POINT ( 'NONE',  ( -3.673772985318163098, 19.25319992234354416, 2.599342558261029001 ) ) ;
#3057 = CARTESIAN_POINT ( 'NONE',  ( 0.05938372350920110426, 27.62819992234354061, -3.680117784833935701 ) ) ;
#3058 = CARTESIAN_POINT ( 'NONE',  ( 0.05938372350921204690, 15.12819992234354771, -2.628655560595669183 ) ) ;
#3059 = ORIENTED_EDGE ( 'NONE', *, *, #5126, .T. ) ;
#3060 = CARTESIAN_POINT ( 'NONE',  ( -1.336863392178569088, 35.00319992234354771, -4.297206761780648421 ) ) ;
#3061 = EDGE_CURVE ( 'NONE', #2915, #17169, #5038, .T. ) ;
#3062 = CARTESIAN_POINT ( 'NONE',  ( -4.000000000000004441, -25.59305773644543081, -8.242876418240973280 ) ) ;
#3063 = ORIENTED_EDGE ( 'NONE', *, *, #16478, .T. ) ;
#3064 = DIRECTION ( 'NONE',  ( -0.000000000000000000, -1.000000000000000000, -0.000000000000000000 ) ) ;
#3065 = CARTESIAN_POINT ( 'NONE',  ( -3.500000000000000444, 32.99680007765648071, 0.05647727720536892260 ) ) ;
#3066 = CARTESIAN_POINT ( 'NONE',  ( -7.425558702535789202, -12.48286535448649914, 8.644520698117755586 ) ) ;
#3067 = CARTESIAN_POINT ( 'NONE',  ( -5.330712181944246111E-15, -25.49437859686066687, -3.585285685531713451 ) ) ;
#3068 = CARTESIAN_POINT ( 'NONE',  ( 2.829195390882805583, 32.12180007765646650, 3.793023760679204770 ) ) ;
#3069 = CARTESIAN_POINT ( 'NONE',  ( 4.000000000000000000, 3.518949890710770134, -4.119968255444916849E-15 ) ) ;
#3070 = ORIENTED_EDGE ( 'NONE', *, *, #10734, .F. ) ;
#3071 = ORIENTED_EDGE ( 'NONE', *, *, #11068, .T. ) ;
#3072 = CARTESIAN_POINT ( 'NONE',  ( 3.518350579753631191, 21.87180007765647360, 1.080741659609802285 ) ) ;
#3073 = EDGE_CURVE ( 'NONE', #9202, #3078, #9631, .T. ) ;
#3074 = CARTESIAN_POINT ( 'NONE',  ( -5.577813053751546416E-15, -26.41867827504920996, -6.474515469367432274 ) ) ;
#3075 = DIRECTION ( 'NONE',  ( -0.000000000000000000, -1.000000000000000000, -0.000000000000000000 ) ) ;
#3076 = CYLINDRICAL_SURFACE ( 'NONE', #63, 4.000000000000000000 ) ;
#3077 = CARTESIAN_POINT ( 'NONE',  ( 1.071796769724485454, -21.55469969778287975, -13.47560852437699452 ) ) ;
#3078 = VERTEX_POINT ( 'NONE', #1215 ) ;
#3079 = CARTESIAN_POINT ( 'NONE',  ( -3.518350579753605434, 21.87819992234354771, 1.080741659609877781 ) ) ;
#3080 = CARTESIAN_POINT ( 'NONE',  ( 4.299564228933482956E-15, -22.38202853593239183, -14.65715655550049590 ) ) ;
#3081 = CARTESIAN_POINT ( 'NONE',  ( 4.243569643750003451, -20.16183871397784344, -8.784099815843886105 ) ) ;
#3082 = CARTESIAN_POINT ( 'NONE',  ( 1.027846397803542144, 36.24680007765648071, -3.346150245485522312 ) ) ;
#3083 = CARTESIAN_POINT ( 'NONE',  ( -2.211161402132839182, 34.12819992234355482, 2.942372952327218627 ) ) ;
#3084 = DIRECTION ( 'NONE',  ( 0.000000000000000000, 0.000000000000000000, 1.000000000000000000 ) ) ;
#3085 = CARTESIAN_POINT ( 'NONE',  ( 4.713407268011036227E-15, -23.35926451522188430, -17.13164280311214327 ) ) ;
#3086 = CARTESIAN_POINT ( 'NONE',  ( -2.121784821875005722, -25.31900764242513091, -5.470575062334849470 ) ) ;
#3087 =( GEOMETRIC_REPRESENTATION_CONTEXT ( 3 ) GLOBAL_UNCERTAINTY_ASSIGNED_CONTEXT ( ( #9521 ) ) GLOBAL_UNIT_ASSIGNED_CONTEXT ( ( #13827, #5206, #8074 ) ) REPRESENTATION_CONTEXT ( 'NONE', 'WORKASPACE' ) );
#3088 = CARTESIAN_POINT ( 'NONE',  ( 8.500000000000019540, 10.00000000000000000, 20.49999999999998934 ) ) ;
#3089 = CARTESIAN_POINT ( 'NONE',  ( -8.767957691171661239, -10.00000000000000178, -4.386791830708038908 ) ) ;
#3090 = EDGE_CURVE ( 'NONE', #15689, #12253, #10419, .T. ) ;
#3091 = CYLINDRICAL_SURFACE ( 'NONE', #10373, 5.000000000000000000 ) ;
#3092 = EDGE_CURVE ( 'NONE', #10922, #526, #18147, .T. ) ;
#3093 = CARTESIAN_POINT ( 'NONE',  ( -1.661723472263481630E-14, -21.54317299706404754, -13.45914668972107897 ) ) ;
#3094 = CARTESIAN_POINT ( 'NONE',  ( -4.243569643750005227, -22.75612477167838676, -3.946144054785039490 ) ) ;
#3095 = LINE ( 'NONE', #15704, #7079 ) ;
#3096 = DIRECTION ( 'NONE',  ( 0.000000000000000000, 0.000000000000000000, 1.000000000000000000 ) ) ;
#3097 = EDGE_CURVE ( 'NONE', #11177, #2571, #18280, .T. ) ;
#3098 = EDGE_LOOP ( 'NONE', ( #17464, #3426, #5820, #17938 ) ) ;
#3099 = CARTESIAN_POINT ( 'NONE',  ( -2.055738996568281518, 21.75319992234354416, 1.423772053676066962 ) ) ;
#3100 = CARTESIAN_POINT ( 'NONE',  ( -4.243569643750000786, -26.96531553179811169, -14.22898156048881724 ) ) ;
#3101 = CARTESIAN_POINT ( 'NONE',  ( -8.500000000000005329, 0.000000000000000000, -22.50000000000000000 ) ) ;
#3102 = PRESENTATION_LAYER_ASSIGNMENT (  '', '', ( #6355 ) ) ;
#3103 = CARTESIAN_POINT ( 'NONE',  ( 3.607379964056306676, 16.49680007765647716, -2.690724712371305838 ) ) ;
#3104 = ADVANCED_FACE ( 'NONE', ( #16890 ), #13624, .F. ) ;
#3105 = DIRECTION ( 'NONE',  ( -3.469446951953613696E-16, -0.000000000000000000, -1.000000000000000000 ) ) ;
#3106 = CARTESIAN_POINT ( 'NONE',  ( 9.000000000000007105, -10.00000000000000178, -3.713574246709336002 ) ) ;
#3107 = VERTEX_POINT ( 'NONE', #5553 ) ;
#3108 = CARTESIAN_POINT ( 'NONE',  ( 4.243569643749997233, -22.70235198077049432, -3.869348550632942363 ) ) ;
#3109 = CARTESIAN_POINT ( 'NONE',  ( -2.115076519116362519, 35.12180007765645939, 3.012182706137107147 ) ) ;
#3110 = CARTESIAN_POINT ( 'NONE',  ( -4.243569643750000786, -26.99757920634285924, -14.27505886298007276 ) ) ;
#3111 = APPLICATION_CONTEXT ( 'automotive_design' ) ;
#3112 = CARTESIAN_POINT ( 'NONE',  ( -4.000000000000004441, -26.10927652916136310, -8.980113258101068752 ) ) ;
#3113 = CARTESIAN_POINT ( 'NONE',  ( -2.121784821875005722, -28.12594732781803941, -9.479300379074118155 ) ) ;
#3114 = DIRECTION ( 'NONE',  ( 0.000000000000000000, 1.000000000000000000, 0.000000000000000000 ) ) ;
#3115 = DIRECTION ( 'NONE',  ( 0.000000000000000000, 0.000000000000000000, 1.000000000000000000 ) ) ;
#3116 = CARTESIAN_POINT ( 'NONE',  ( 1.999999999999994449, -28.86191761092706187, -10.89813317876196308 ) ) ;
#3117 = CARTESIAN_POINT ( 'NONE',  ( 2.121784821874994176, -27.30860090601781209, -8.312008715962296179 ) ) ;
#3118 = FACE_OUTER_BOUND ( 'NONE', #16048, .T. ) ;
#3119 = CARTESIAN_POINT ( 'NONE',  ( -4.000000000000000888, -20.43192143683950590, -4.898327806512866367 ) ) ;
#3120 = CARTESIAN_POINT ( 'NONE',  ( 0.05938372350926800214, 24.87180007765647716, 2.628655560595669183 ) ) ;
#3121 = ORIENTED_EDGE ( 'NONE', *, *, #7037, .T. ) ;
#3122 = CARTESIAN_POINT ( 'NONE',  ( 2.211161402132902243, 19.62180007765647716, 2.942372952327172442 ) ) ;
#3123 = DIRECTION ( 'NONE',  ( 0.000000000000000000, 0.000000000000000000, -1.000000000000000000 ) ) ;
#3124 = DIRECTION ( 'NONE',  ( 0.000000000000000000, -1.000000000000000000, 0.000000000000000000 ) ) ;
#3125 = CARTESIAN_POINT ( 'NONE',  ( -5.577813053751546416E-15, -26.22509622848567545, -6.198051655426662698 ) ) ;
#3126 = CARTESIAN_POINT ( 'NONE',  ( 3.481649420246394122, 18.37819992234354771, 1.193696214020467439 ) ) ;
#3127 = ORIENTED_EDGE ( 'NONE', *, *, #8075, .F. ) ;
#3128 = CARTESIAN_POINT ( 'NONE',  ( -4.243569643750000786, -24.41648524276317289, -10.58887466367959540 ) ) ;
#3129 = CARTESIAN_POINT ( 'NONE',  ( 4.518350579753633411, 34.37180007765647360, 1.405661355842698468 ) ) ;
#3130 = VERTEX_POINT ( 'NONE', #1029 ) ;
#3131 = CARTESIAN_POINT ( 'NONE',  ( 4.730628863548789710E-15, -21.75767183597312737, -15.33467581975593141 ) ) ;
#3132 = CARTESIAN_POINT ( 'NONE',  ( 1.071796769724495224, -18.71549633784523081, -9.420805905146465875 ) ) ;
#3133 = CARTESIAN_POINT ( 'NONE',  ( 2.694913683823408235, -10.54254386713301805, 22.30101802474215233 ) ) ;
#3134 = CARTESIAN_POINT ( 'NONE',  ( -1.734723475976807094E-15, 25.39999999999999503, -2.500000000000000000 ) ) ;
#3135 = CARTESIAN_POINT ( 'NONE',  ( 2.121784821875004390, -18.65290254502614431, -8.764860689675106897 ) ) ;
#3136 = VERTEX_POINT ( 'NONE', #16619 ) ;
#3137 = CARTESIAN_POINT ( 'NONE',  ( 4.000000000000003553, -20.38995483025674105, -8.864711188050506507 ) ) ;
#3138 = DIRECTION ( 'NONE',  ( -3.469446951953613696E-16, -0.000000000000000000, -1.000000000000000000 ) ) ;
#3139 = ORIENTED_EDGE ( 'NONE', *, *, #17076, .T. ) ;
#3140 = ORIENTED_EDGE ( 'NONE', *, *, #4221, .T. ) ;
#3141 =( BOUNDED_CURVE ( )  B_SPLINE_CURVE ( 2, ( #7426, #3456, #400, #7609, #7330, #9097, #6325, #5946, #6038 ),
 .UNSPECIFIED., .F., .T. ) 
 B_SPLINE_CURVE_WITH_KNOTS ( ( 3, 2, 2, 2, 3 ),
 ( 0.9568965517241379004, 0.9597701149425287293, 0.9655172413793103869, 0.9712643678160919336, 0.9741379310344827624 ),
 .UNSPECIFIED. ) 
 CURVE ( )  GEOMETRIC_REPRESENTATION_ITEM ( )  RATIONAL_B_SPLINE_CURVE ( ( 0.9330127018922194093, 0.9330127018922194093, 1.000000000000000000, 0.8660254037844387076, 1.000000000000000000, 0.8660254037844387076, 1.000000000000000000, 0.9330127018922194093, 0.9330127018922194093 ) ) 
 REPRESENTATION_ITEM ( '' )  );
#3142 = AXIS2_PLACEMENT_3D ( 'NONE', #1145, #9835, #5590 ) ;
#3143 = CARTESIAN_POINT ( 'NONE',  ( -4.000000000000000888, -20.43192143683950590, -4.898327806512866367 ) ) ;
#3144 = ADVANCED_FACE ( 'NONE', ( #3893 ), #4255, .T. ) ;
#3145 = DIRECTION ( 'NONE',  ( -0.000000000000000000, -1.000000000000000000, -0.000000000000000000 ) ) ;
#3146 =( NAMED_UNIT ( * ) SI_UNIT ( $, .STERADIAN. ) SOLID_ANGLE_UNIT ( ) );
#3147 = CARTESIAN_POINT ( 'NONE',  ( -2.829195390882724315, 29.12819992234354416, 3.793023760679264722 ) ) ;
#3148 = B_SPLINE_CURVE_WITH_KNOTS ( 'NONE', 3,
 ( #10112, #7335, #11880, #3370, #15983, #15883, #9103, #3279, #6233, #5858, #8914, #13274, #17578, #9014 ),
 .UNSPECIFIED., .F., .F.,
 ( 4, 2, 2, 2, 2, 2, 4 ),
 ( 0.000000000000000000, 0.004344441487376424042, 0.008688882974752848085, 0.01086110371844106227, 0.01303332446212927473, 0.01520554520581748718, 0.01737776594950569964 ),
 .UNSPECIFIED. ) ;
#3149 = CARTESIAN_POINT ( 'NONE',  ( -2.115076519116425580, 29.87819992234354061, -3.012182706137063182 ) ) ;
#3150 = CIRCLE ( 'NONE', #13497, 10.00000000000000178 ) ;
#3151 = CARTESIAN_POINT ( 'NONE',  ( -2.481649420246374138, 35.37180007765647360, 0.8687765177876256573 ) ) ;
#3152 = ORIENTED_EDGE ( 'NONE', *, *, #3822, .T. ) ;
#3153 = CARTESIAN_POINT ( 'NONE',  ( -2.829195390882724315, 31.62819992234354416, 3.793023760679264722 ) ) ;
#3154 = CARTESIAN_POINT ( 'NONE',  ( -5.279047395330986450E-15, -26.66746192775513080, -5.750966715416751640 ) ) ;
#3155 = ORIENTED_EDGE ( 'NONE', *, *, #15116, .F. ) ;
#3156 = CARTESIAN_POINT ( 'NONE',  ( 4.898587196589413815E-16, 2.700915433685006750, 35.11257424290206330 ) ) ;
#3157 = CARTESIAN_POINT ( 'NONE',  ( -1.135272562821090014, 30.99680007765647716, -3.311245368580554072 ) ) ;
#3158 = CARTESIAN_POINT ( 'NONE',  ( -7.666554591372073624, -10.31261801969990444, 7.182588619990075252 ) ) ;
#3159 = CARTESIAN_POINT ( 'NONE',  ( -2.121784821874996396, -19.09383943047100018, -9.394583823722271632 ) ) ;
#3160 = CIRCLE ( 'NONE', #11421, 0.9999999999999991118 ) ;
#3161 = CARTESIAN_POINT ( 'NONE',  ( -1.336863392178478716, 29.99680007765647716, 4.297206761780677731 ) ) ;
#3162 = CARTESIAN_POINT ( 'NONE',  ( -1.734723475976807094E-15, 43.00000000000000000, -11.50000000000000178 ) ) ;
#3163 = EDGE_CURVE ( 'NONE', #13322, #2431, #10104, .T. ) ;
#3164 = EDGE_LOOP ( 'NONE', ( #10718, #1710, #1953, #11361 ) ) ;
#3165 = EDGE_LOOP ( 'NONE', ( #15403, #364, #9885, #13609, #4187 ) ) ;
#3166 = CARTESIAN_POINT ( 'NONE',  ( 3.518350579753631191, 31.87180007765647716, 1.080741659609802285 ) ) ;
#3167 = DIRECTION ( 'NONE',  ( 0.000000000000000000, 0.000000000000000000, -1.000000000000000000 ) ) ;
#3168 = CARTESIAN_POINT ( 'NONE',  ( 4.299564228933482956E-15, -22.89824732864832768, -15.39439339536058959 ) ) ;
#3169 = CARTESIAN_POINT ( 'NONE',  ( 9.000000000000000000, 34.19999999999999574, -2.500000000000001332 ) ) ;
#3170 = ORIENTED_EDGE ( 'NONE', *, *, #10062, .T. ) ;
#3171 = CARTESIAN_POINT ( 'NONE',  ( -1.135272562821019626, 21.50319992234354416, 3.311245368580577164 ) ) ;
#3172 = LINE ( 'NONE', #1264, #2479 ) ;
#3173 = CARTESIAN_POINT ( 'NONE',  ( -4.243569643749997233, -19.30147405945127304, -7.555371749410396021 ) ) ;
#3174 = CARTESIAN_POINT ( 'NONE',  ( -2.481649420246374138, 17.87180007765647716, 0.8687765177876256573 ) ) ;
#3175 = CARTESIAN_POINT ( 'NONE',  ( -3.518350579753605434, 36.87819992234354771, 1.080741659609877781 ) ) ;
#3176 = CARTESIAN_POINT ( 'NONE',  ( 2.121784821874994176, -29.92195854414224598, -12.04427021775403084 ) ) ;
#3177 = CIRCLE ( 'NONE', #3472, 0.9999999999999991118 ) ;
#3178 = CARTESIAN_POINT ( 'NONE',  ( 3.999999999999996447, -28.86244342364637205, -12.91204307068823987 ) ) ;
#3179 = CARTESIAN_POINT ( 'NONE',  ( -4.243569643749997233, -20.36617531942789228, -9.075922731621842487 ) ) ;
#3180 = CARTESIAN_POINT ( 'NONE',  ( 3.579096709490575479E-14, -25.12813129325936501, -4.631423369717193594 ) ) ;
#3181 = CARTESIAN_POINT ( 'NONE',  ( -3.820650143297558365, -10.00000000000057199, -3.109998371641696124 ) ) ;
#3182 = CARTESIAN_POINT ( 'NONE',  ( 0.000000000000000000, 9.254131787996968228, 30.52396275209373044 ) ) ;
#3183 = AXIS2_PLACEMENT_3D ( 'NONE', #2698, #11198, #2786 ) ;
#3184 = DIRECTION ( 'NONE',  ( 0.000000000000000000, -1.000000000000000000, 0.000000000000000000 ) ) ;
#3185 = VERTEX_POINT ( 'NONE', #10264 ) ;
#3186 = AXIS2_PLACEMENT_3D ( 'NONE', #4405, #2841, #1543 ) ;
#3187 = EDGE_LOOP ( 'NONE', ( #4711, #16801, #170, #9428 ) ) ;
#3188 = CARTESIAN_POINT ( 'NONE',  ( 2.121784821874994176, -23.69506935700625050, -3.151350836941627875 ) ) ;
#3189 = CARTESIAN_POINT ( 'NONE',  ( -9.000000000000001776, 31.99999999999999289, 2.499999999999995559 ) ) ;
#3190 = FACE_OUTER_BOUND ( 'NONE', #10306, .T. ) ;
#3191 = VERTEX_POINT ( 'NONE', #2961 ) ;
#3192 = CARTESIAN_POINT ( 'NONE',  ( -2.500000000000001332, 22.00319992234354771, -0.05647727720530596601 ) ) ;
#3193 = DIRECTION ( 'NONE',  ( 0.000000000000000000, -1.000000000000000000, 0.000000000000000000 ) ) ;
#3194 = CARTESIAN_POINT ( 'NONE',  ( 3.500000000000000444, 16.74680007765647716, -0.05647727720536935281 ) ) ;
#3195 = DIRECTION ( 'NONE',  ( 0.000000000000000000, 0.000000000000000000, -1.000000000000000000 ) ) ;
#3196 = CYLINDRICAL_SURFACE ( 'NONE', #12014, 4.000000000000000000 ) ;
#3197 = EDGE_CURVE ( 'NONE', #269, #11442, #11301, .T. ) ;
#3198 = VERTEX_POINT ( 'NONE', #2870 ) ;
#3199 = CARTESIAN_POINT ( 'NONE',  ( -2.798362969681365886, 40.24680007765648071, 2.102939460078824929 ) ) ;
#3200 = CARTESIAN_POINT ( 'NONE',  ( 4.243569643750000786, -27.12663390452184942, -14.45936807294509308 ) ) ;
#3201 = EDGE_CURVE ( 'NONE', #6301, #8381, #15753, .T. ) ;
#3202 = AXIS2_PLACEMENT_3D ( 'NONE', #8544, #15351, #17105 ) ;
#3203 = EDGE_CURVE ( 'NONE', #7786, #17921, #2149, .T. ) ;
#3204 = CYLINDRICAL_SURFACE ( 'NONE', #3981, 4.000000000000000000 ) ;
#3205 = CARTESIAN_POINT ( 'NONE',  ( 4.243569643749997233, -28.09038562974308562, -11.56425806667268752 ) ) ;
#3206 = DIRECTION ( 'NONE',  ( 0.000000000000000000, 0.000000000000000000, -1.000000000000000000 ) ) ;
#3207 = ADVANCED_FACE ( 'NONE', ( #17066 ), #4491, .T. ) ;
#3208 = CARTESIAN_POINT ( 'NONE',  ( -4.000000000000000888, -24.56167177856700334, -10.79622252539362925 ) ) ;
#3209 = DIRECTION ( 'NONE',  ( 0.000000000000000000, 0.000000000000000000, 1.000000000000000000 ) ) ;
#3210 = CARTESIAN_POINT ( 'NONE',  ( 4.243569643749996345, -26.28361985523730837, -8.983929127162353367 ) ) ;
#3211 = PLANE ( 'NONE',  #6539 ) ;
#3212 = CARTESIAN_POINT ( 'NONE',  ( -4.000000000000000888, -19.91570264412356650, -4.161090966652770895 ) ) ;
#3213 = AXIS2_PLACEMENT_3D ( 'NONE', #15612, #6977, #14222 ) ;
#3214 = CARTESIAN_POINT ( 'NONE',  ( -2.518350579753628526, 23.12180007765647005, -0.7558219633769075463 ) ) ;
#3215 = AXIS2_PLACEMENT_3D ( 'NONE', #7307, #5749, #181 ) ;
#3216 = AXIS2_PLACEMENT_3D ( 'NONE', #10862, #13548, #6512 ) ;
#3217 = VERTEX_POINT ( 'NONE', #6005 ) ;
#3218 = CARTESIAN_POINT ( 'NONE',  ( -2.115076519116362519, 22.62180007765647716, 3.012182706137108035 ) ) ;
#3219 = CARTESIAN_POINT ( 'NONE',  ( 2.000000000000004441, -21.03575413528086102, -11.80016713181543331 ) ) ;
#3220 = CARTESIAN_POINT ( 'NONE',  ( 4.000000000000003553, -24.84234191813664339, -15.22337893285059529 ) ) ;
#3221 = FACE_OUTER_BOUND ( 'NONE', #16383, .T. ) ;
#3222 = CARTESIAN_POINT ( 'NONE',  ( 0.05938372350920109732, 20.12819992234353705, -3.680117784833935701 ) ) ;
#3223 = ORIENTED_EDGE ( 'NONE', *, *, #4672, .T. ) ;
#3224 = CARTESIAN_POINT ( 'NONE',  ( 2.121784821875004390, -20.45966831953192511, -11.34518962918543927 ) ) ;
#3225 = CARTESIAN_POINT ( 'NONE',  ( -2.733110507866247652, 40.12180007765647360, 3.862833514489154574 ) ) ;
#3226 = ORIENTED_EDGE ( 'NONE', *, *, #12932, .T. ) ;
#3227 = CIRCLE ( 'NONE', #1748, 8.000000000000003553 ) ;
#3228 = CARTESIAN_POINT ( 'NONE',  ( 0.000000000000000000, 3.518949890710770134, -4.119968255444916849E-15 ) ) ;
#3229 = CARTESIAN_POINT ( 'NONE',  ( -5.577813053751546416E-15, -23.38589286854802296, -2.143249036196138047 ) ) ;
#3230 = CARTESIAN_POINT ( 'NONE',  ( 4.730628863548789710E-15, -22.01578123233109707, -15.70329423968597915 ) ) ;
#3231 = DIRECTION ( 'NONE',  ( 0.000000000000000000, 0.000000000000000000, 1.000000000000000000 ) ) ;
#3232 = CARTESIAN_POINT ( 'NONE',  ( 0.000000000000000000, 9.254131787996968228, 30.52396275209373044 ) ) ;
#3233 = DIRECTION ( 'NONE',  ( 0.000000000000000000, 0.000000000000000000, -1.000000000000000000 ) ) ;
#3234 = CARTESIAN_POINT ( 'NONE',  ( -4.243569643750000786, -21.31917248646755070, -6.165453624519022569 ) ) ;
#3235 = ORIENTED_EDGE ( 'NONE', *, *, #10761, .F. ) ;
#3236 = CARTESIAN_POINT ( 'NONE',  ( -1.999999999999996225, -20.73462650619655534, -11.37011230856371036 ) ) ;
#3237 = CARTESIAN_POINT ( 'NONE',  ( -5.577813053751546416E-15, -25.64435008597530796, -5.368660209577289955 ) ) ;
#3238 = DIRECTION ( 'NONE',  ( 1.000000000000000000, 0.000000000000000000, -4.336808689942021680E-16 ) ) ;
#3239 = ORIENTED_EDGE ( 'NONE', *, *, #2688, .F. ) ;
#3240 = ORIENTED_EDGE ( 'NONE', *, *, #9829, .T. ) ;
#3241 = CARTESIAN_POINT ( 'NONE',  ( 1.300000000000000044, 0.7216878364870329410, 1.249999999999999778 ) ) ;
#3242 = LINE ( 'NONE', #3516, #4220 ) ;
#3243 = CIRCLE ( 'NONE', #3812, 1.250000000000000222 ) ;
#3244 = CARTESIAN_POINT ( 'NONE',  ( -1.336863392178569088, 25.00319992234354771, -4.297206761780648421 ) ) ;
#3245 = CARTESIAN_POINT ( 'NONE',  ( -3.481649420246394566, 24.62819992234354061, -1.193696214020467883 ) ) ;
#3246 = CARTESIAN_POINT ( 'NONE',  ( 2.055738996568281518, 20.50319992234355126, -1.423772053676066518 ) ) ;
#3247 = ORIENTED_EDGE ( 'NONE', *, *, #10691, .F. ) ;
#3248 = CARTESIAN_POINT ( 'NONE',  ( -3.607379964056306676, 17.74680007765647716, 2.690724712371306282 ) ) ;
#3249 = CARTESIAN_POINT ( 'NONE',  ( -1.999999999999996225, -18.60522398553836965, -8.329010343134054750 ) ) ;
#3250 = ORIENTED_EDGE ( 'NONE', *, *, #5910, .T. ) ;
#3251 = DIRECTION ( 'NONE',  ( -3.373073425510457965E-16, 0.000000000000000000, -1.000000000000000000 ) ) ;
#3252 = CARTESIAN_POINT ( 'NONE',  ( -2.798362969681365886, 27.74680007765648071, 2.102939460078824929 ) ) ;
#3253 = CARTESIAN_POINT ( 'NONE',  ( -9.320967924960621431, -9.992678415326631480, -2.177024574453123140 ) ) ;
#3254 = AXIS2_PLACEMENT_3D ( 'NONE', #4425, #13043, #17344 ) ;
#3255 = CARTESIAN_POINT ( 'NONE',  ( -4.243569643749998122, -19.30147405945127304, -7.555371749410397797 ) ) ;
#3256 =( BOUNDED_CURVE ( )  B_SPLINE_CURVE ( 2, ( #3168, #4190, #11398, #12619, #5843, #18307, #1685, #11585, #16913 ),
 .UNSPECIFIED., .F., .F. ) 
 B_SPLINE_CURVE_WITH_KNOTS ( ( 3, 2, 2, 2, 3 ),
 ( 0.1120689655172413812, 0.1149425287356321823, 0.1206896551724137984, 0.1264367816091954144, 0.1293103448275862155 ),
 .UNSPECIFIED. ) 
 CURVE ( )  GEOMETRIC_REPRESENTATION_ITEM ( )  RATIONAL_B_SPLINE_CURVE ( ( 0.9330127018922194093, 0.9330127018922194093, 1.000000000000000000, 0.8660254037844387076, 1.000000000000000000, 0.8660254037844387076, 1.000000000000000000, 0.9330127018922194093, 0.9330127018922194093 ) ) 
 REPRESENTATION_ITEM ( '' )  );
#3257 = CARTESIAN_POINT ( 'NONE',  ( 4.499999999999999112, 29.24680007765647716, -0.05647727720537982360 ) ) ;
#3258 = DIRECTION ( 'NONE',  ( 0.000000000000000000, 0.000000000000000000, 1.000000000000000000 ) ) ;
#3259 = ORIENTED_EDGE ( 'NONE', *, *, #9603, .T. ) ;
#3260 = CARTESIAN_POINT ( 'NONE',  ( -0.05938372350927861171, 28.62180007765648071, -3.680117784833935701 ) ) ;
#3261 = DIRECTION ( 'NONE',  ( 0.000000000000000000, 0.000000000000000000, 1.000000000000000000 ) ) ;
#3262 = CARTESIAN_POINT ( 'NONE',  ( -8.500000000000010658, 10.00000000000000000, 22.64999999999998437 ) ) ;
#3263 = DIRECTION ( 'NONE',  ( -4.915049848600951133E-16, 0.000000000000000000, -1.000000000000000000 ) ) ;
#3264 = DIRECTION ( 'NONE',  ( 1.000000000000000000, 0.000000000000000000, 0.000000000000000000 ) ) ;
#3265 = ORIENTED_EDGE ( 'NONE', *, *, #11841, .F. ) ;
#3266 = CARTESIAN_POINT ( 'NONE',  ( -0.05938372350920063936, 28.87819992234353705, 3.680117784833935701 ) ) ;
#3267 = AXIS2_PLACEMENT_3D ( 'NONE', #4851, #7621, #6338 ) ;
#3268 = CARTESIAN_POINT ( 'NONE',  ( 2.000000000000004441, -22.84251990978664182, -14.38049607132576746 ) ) ;
#3269 = CARTESIAN_POINT ( 'NONE',  ( -4.243569643749997233, -20.07580224852517858, -8.661227009200541005 ) ) ;
#3270 = CARTESIAN_POINT ( 'NONE',  ( 1.497042530366477164, 23.87180007765647716, -2.161531897785062384 ) ) ;
#3271 = ADVANCED_FACE ( 'NONE', ( #1393, #15571 ), #1572, .F. ) ;
#3272 = AXIS2_PLACEMENT_3D ( 'NONE', #4866, #10516, #13759 ) ;
#3273 = CARTESIAN_POINT ( 'NONE',  ( 2.864755990943222308, 33.00319992234354771, -2.011557305968548093 ) ) ;
#3274 = CARTESIAN_POINT ( 'NONE',  ( 4.243569643749997233, -28.63886809700377611, -12.34757220902403851 ) ) ;
#3275 = CARTESIAN_POINT ( 'NONE',  ( -4.000000000000000888, -26.82012899599428124, -14.02163369877478161 ) ) ;
#3276 = EDGE_CURVE ( 'NONE', #16215, #8582, #9234, .T. ) ;
#3277 = CARTESIAN_POINT ( 'NONE',  ( -5.330712181944245322E-15, -27.07529864955322552, -5.843073507603255834 ) ) ;
#3278 = ADVANCED_FACE ( 'NONE', ( #7117 ), #7208, .F. ) ;
#3279 = CARTESIAN_POINT ( 'NONE',  ( -7.381432656702920703, -13.34861180364788247, 2.835002125509740623 ) ) ;
#3280 = CARTESIAN_POINT ( 'NONE',  ( -7.649231854195242875, -10.00000000000000178, -6.849627928939406196 ) ) ;
#3281 = CARTESIAN_POINT ( 'NONE',  ( 1.071796769724485232, -23.56794821439272880, -2.403251015480991626 ) ) ;
#3282 = CARTESIAN_POINT ( 'NONE',  ( 0.000000000000000000, 5.977523610840987267, 32.81826849749789687 ) ) ;
#3283 = ORIENTED_EDGE ( 'NONE', *, *, #11462, .T. ) ;
#3284 = EDGE_LOOP ( 'NONE', ( #9897, #4410, #14663, #13878 ) ) ;
#3285 = CARTESIAN_POINT ( 'NONE',  ( 4.898587196589413815E-16, 2.700915433685006750, 35.11257424290206330 ) ) ;
#3286 = ORIENTED_EDGE ( 'NONE', *, *, #17047, .F. ) ;
#3287 = CARTESIAN_POINT ( 'NONE',  ( -1.497042530366522461, 24.87819992234354771, -2.161531897785030409 ) ) ;
#3288 = FILL_AREA_STYLE_COLOUR ( '', #4181 ) ;
#3289 = CARTESIAN_POINT ( 'NONE',  ( 4.730628863548789710E-15, -21.20918936871244043, -14.55136167740457864 ) ) ;
#3290 = CARTESIAN_POINT ( 'NONE',  ( 8.500000000000001776, 15.00000000000000000, -18.29999999999999716 ) ) ;
#3291 = CARTESIAN_POINT ( 'NONE',  ( 10.00000000000000000, 43.00000000000000000, -2.500000000000003109 ) ) ;
#3292 = CARTESIAN_POINT ( 'NONE',  ( 1.448116719718851364, -9.999999999999500844, -4.839896329769187489 ) ) ;
#3293 = ORIENTED_EDGE ( 'NONE', *, *, #13111, .T. ) ;
#3294 = CARTESIAN_POINT ( 'NONE',  ( 0.05938372350927906274, 37.37180007765645939, 3.680117784833935701 ) ) ;
#3295 = CARTESIAN_POINT ( 'NONE',  ( 4.000000000000000888, -19.98022999250811793, -4.253245570628513939 ) ) ;
#3296 = DIRECTION ( 'NONE',  ( 1.000000000000000000, 0.000000000000000000, -0.000000000000000000 ) ) ;
#3297 = CARTESIAN_POINT ( 'NONE',  ( -4.243569643750004339, -25.59532813161605347, -8.000946674015564142 ) ) ;
#3298 = CARTESIAN_POINT ( 'NONE',  ( 0.000000000000000000, -10.00099999999999767, 0.000000000000000000 ) ) ;
#3299 = DIRECTION ( 'NONE',  ( 1.000000000000000000, 0.000000000000000000, 0.000000000000000000 ) ) ;
#3300 = DIRECTION ( 'NONE',  ( 0.000000000000000000, 0.000000000000000000, 1.000000000000000000 ) ) ;
#3301 = CARTESIAN_POINT ( 'NONE',  ( -4.243569643750005227, -24.82099994254214437, -6.895091414225420934 ) ) ;
#3302 = DIRECTION ( 'NONE',  ( -3.469446951953616654E-16, 0.000000000000000000, -1.000000000000000000 ) ) ;
#3303 = DIRECTION ( 'NONE',  ( 3.469446951953612217E-16, -0.000000000000000000, 1.000000000000000000 ) ) ;
#3304 = CARTESIAN_POINT ( 'NONE',  ( 2.500000000000001332, 19.24680007765648071, -0.05647727720535888202 ) ) ;
#3305 = LINE ( 'NONE', #1930, #8519 ) ;
#3306 = CARTESIAN_POINT ( 'NONE',  ( 1.027846397803542144, 23.74680007765647716, -3.346150245485522312 ) ) ;
#3307 = ADVANCED_FACE ( 'NONE', ( #12777 ), #171, .F. ) ;
#3308 = CARTESIAN_POINT ( 'NONE',  ( 1.999999999999994449, -27.31326123277925433, -8.686422659181676664 ) ) ;
#3309 = DIRECTION ( 'NONE',  ( 1.000000000000000000, 0.000000000000000000, 0.000000000000000000 ) ) ;
#3310 = CARTESIAN_POINT ( 'NONE',  ( -3.999999999999997335, -24.24008665996804268, -14.36326928634715472 ) ) ;
#3311 = DIRECTION ( 'NONE',  ( 0.000000000000000000, 0.000000000000000000, -1.000000000000000000 ) ) ;
#3312 = CARTESIAN_POINT ( 'NONE',  ( -2.115076519116425580, 14.87819992234354594, -3.012182706137062738 ) ) ;
#3313 = EDGE_LOOP ( 'NONE', ( #5304, #9111, #889, #9369 ) ) ;
#3314 = CARTESIAN_POINT ( 'NONE',  ( -2.121784821874996396, -20.41665008680558913, -11.28375322586376939 ) ) ;
#3315 = CARTESIAN_POINT ( 'NONE',  ( 3.518350579753631191, 19.37180007765648071, 1.080741659609802285 ) ) ;
#3316 = AXIS2_PLACEMENT_3D ( 'NONE', #14974, #15248, #2270 ) ;
#3317 = EDGE_LOOP ( 'NONE', ( #16483, #11941, #1266, #4428 ) ) ;
#3318 = CARTESIAN_POINT ( 'NONE',  ( 1.999999999999994449, -24.40953052304715953, -4.539465433961872520 ) ) ;
#3319 = DIRECTION ( 'NONE',  ( 0.000000000000000000, 0.000000000000000000, -1.000000000000000000 ) ) ;
#3320 = CARTESIAN_POINT ( 'NONE',  ( -2.121784821874996396, -21.96530646495340378, -13.49546374544405403 ) ) ;
#3321 = CARTESIAN_POINT ( 'NONE',  ( -5.577813053751546416E-15, -28.54808079570739920, -9.515617434797091434 ) ) ;
#3322 = LINE ( 'NONE', #17435, #1778 ) ;
#3323 = CARTESIAN_POINT ( 'NONE',  ( 3.579096709490575479E-14, -25.90245948233327056, -5.737278629507336802 ) ) ;
#3324 = CARTESIAN_POINT ( 'NONE',  ( -4.243569643750000786, -21.06106309010958100, -5.796835204588974833 ) ) ;
#3325 = EDGE_CURVE ( 'NONE', #3191, #13521, #5103, .T. ) ;
#3326 = ORIENTED_EDGE ( 'NONE', *, *, #14028, .T. ) ;
#3327 = LINE ( 'NONE', #1949, #9788 ) ;
#3328 = EDGE_CURVE ( 'NONE', #16052, #14634, #10434, .T. ) ;
#3329 = DIRECTION ( 'NONE',  ( -0.000000000000000000, -1.000000000000000000, -0.000000000000000000 ) ) ;
#3330 = AXIS2_PLACEMENT_3D ( 'NONE', #296, #5844, #2811 ) ;
#3331 = CARTESIAN_POINT ( 'NONE',  ( 8.000000000000000000, 29.79999999999999716, -2.500000000000000888 ) ) ;
#3332 = EDGE_CURVE ( 'NONE', #2342, #8991, #10075, .T. ) ;
#3333 = VERTEX_POINT ( 'NONE', #5915 ) ;
#3334 = ORIENTED_EDGE ( 'NONE', *, *, #14608, .T. ) ;
#3335 = CARTESIAN_POINT ( 'NONE',  ( 10.00000000000000000, 29.79999999999999716, -2.500000000000003109 ) ) ;
#3336 = DIRECTION ( 'NONE',  ( 0.000000000000000000, 0.000000000000000000, -1.000000000000000000 ) ) ;
#3337 = CARTESIAN_POINT ( 'NONE',  ( 3.607379964056363075, 28.50319992234354416, 2.690724712371229010 ) ) ;
#3338 = CARTESIAN_POINT ( 'NONE',  ( 3.481649420246395010, 38.37819992234354061, 1.193696214020467439 ) ) ;
#3339 = CARTESIAN_POINT ( 'NONE',  ( -0.05938372350921170689, 16.37819992234354416, 2.628655560595669183 ) ) ;
#3340 = ORIENTED_EDGE ( 'NONE', *, *, #12040, .T. ) ;
#3341 = CARTESIAN_POINT ( 'NONE',  ( 3.607379964056306676, 16.49680007765647716, -2.690724712371305838 ) ) ;
#3342 = CARTESIAN_POINT ( 'NONE',  ( -3.999999999999997335, -19.78769957208813679, -8.004601541547065935 ) ) ;
#3343 = EDGE_LOOP ( 'NONE', ( #4756, #16088, #10073, #5139 ) ) ;
#3344 = AXIS2_PLACEMENT_3D ( 'NONE', #14936, #2228, #7855 ) ;
#3345 = DIRECTION ( 'NONE',  ( -3.373073425510457965E-16, 0.000000000000000000, -1.000000000000000000 ) ) ;
#3346 = CIRCLE ( 'NONE', #17284, 2.499999999999999556 ) ;
#3347 = CARTESIAN_POINT ( 'NONE',  ( -3.518350579753630747, 28.12180007765647360, -1.080741659609802729 ) ) ;
#3348 = CARTESIAN_POINT ( 'NONE',  ( 8.399999999999998579, 0.000000000000000000, -4.400000000000002132 ) ) ;
#3349 = CARTESIAN_POINT ( 'NONE',  ( 4.730628863548789710E-15, -17.85376721605885209, -9.759322218313958075 ) ) ;
#3350 = CARTESIAN_POINT ( 'NONE',  ( -1.444289557196047014, 28.49680007765648071, -4.262301884875704161 ) ) ;
#3351 = DIRECTION ( 'NONE',  ( 0.000000000000000000, 1.000000000000000000, 0.000000000000000000 ) ) ;
#3352 = VERTEX_POINT ( 'NONE', #11561 ) ;
#3353 = CARTESIAN_POINT ( 'NONE',  ( -3.518350579753630747, 30.62180007765647716, -1.080741659609802729 ) ) ;
#3354 = CARTESIAN_POINT ( 'NONE',  ( 3.579096709490575479E-14, -23.06325612239561451, -1.682476010276811040 ) ) ;
#3355 = CARTESIAN_POINT ( 'NONE',  ( 8.000000000000000000, 13.00000000000000178, 2.500000000000000000 ) ) ;
#3356 = CIRCLE ( 'NONE', #13403, 0.9999999999999991118 ) ;
#3357 = CARTESIAN_POINT ( 'NONE',  ( 3.999999999999996447, 6.938893903907228378E-15, 24.28148006742132026 ) ) ;
#3358 =( NAMED_UNIT ( * ) SI_UNIT ( $, .STERADIAN. ) SOLID_ANGLE_UNIT ( ) );
#3359 = EDGE_LOOP ( 'NONE', ( #5671, #3956, #13155, #10290 ) ) ;
#3360 = MECHANICAL_DESIGN_GEOMETRIC_PRESENTATION_REPRESENTATION (  '', ( #1885 ), #7184 ) ;
#3361 = CARTESIAN_POINT ( 'NONE',  ( 3.500000000000000444, 28.25319992234354416, 0.05647727720529520379 ) ) ;
#3362 = CARTESIAN_POINT ( 'NONE',  ( 4.898587196589413815E-16, 2.700915433685006750, 35.11257424290206330 ) ) ;
#3363 = CARTESIAN_POINT ( 'NONE',  ( -5.330712181944245322E-15, -25.75248799321863657, -3.953904105461760743 ) ) ;
#3364 = CARTESIAN_POINT ( 'NONE',  ( -0.8262555684461330152, 18.49680007765647716, -2.360188852285403982 ) ) ;
#3365 = EDGE_CURVE ( 'NONE', #14905, #4281, #13321, .T. ) ;
#3366 = CARTESIAN_POINT ( 'NONE',  ( 1.444289557195957086, 20.25319992234354416, -4.262301884875733471 ) ) ;
#3367 = CARTESIAN_POINT ( 'NONE',  ( -4.243569643749998122, -24.49592566115538972, -14.97381745050260804 ) ) ;
#3368 = CARTESIAN_POINT ( 'NONE',  ( -1.999999999999996225, -22.99308372362383679, -14.59552348194486626 ) ) ;
#3369 = CARTESIAN_POINT ( 'NONE',  ( -4.243569643749997233, -19.33373773399602058, -7.601449051901653320 ) ) ;
#3370 = CARTESIAN_POINT ( 'NONE',  ( -7.429936681370006291, -12.48975054434458620, 8.592747494639136008 ) ) ;
#3371 = TOROIDAL_SURFACE ( 'NONE', #13719, 9.000000000000003553, 0.9999999999999991118 ) ;
#3372 = FACE_OUTER_BOUND ( 'NONE', #11938, .T. ) ;
#3373 = CARTESIAN_POINT ( 'NONE',  ( -9.000000000000001776, 34.19999999999999574, 2.499999999999998224 ) ) ;
#3374 = CARTESIAN_POINT ( 'NONE',  ( 8.673617379884035472E-15, 13.00000000000000178, 3.469446951953614189E-15 ) ) ;
#3375 = ORIENTED_EDGE ( 'NONE', *, *, #17613, .T. ) ;
#3376 = ORIENTED_EDGE ( 'NONE', *, *, #1981, .F. ) ;
#3377 = CARTESIAN_POINT ( 'NONE',  ( 20.00000000000000355, 0.000000000000000000, 3.309499999999999886 ) ) ;
#3378 = EDGE_CURVE ( 'NONE', #6052, #11658, #13147, .T. ) ;
#3379 = CARTESIAN_POINT ( 'NONE',  ( 4.000000000000003553, -23.74537698291033294, -13.65675064714112708 ) ) ;
#3380 = LINE ( 'NONE', #9021, #12370 ) ;
#3381 = ORIENTED_EDGE ( 'NONE', *, *, #14211, .F. ) ;
#3382 = CARTESIAN_POINT ( 'NONE',  ( -2.500000000000001332, 27.00319992234355126, -0.05647727720530596601 ) ) ;
#3383 = CARTESIAN_POINT ( 'NONE',  ( -4.648177544792955347E-16, -29.77410042770280185, -11.26655492845805107 ) ) ;
#3384 = CARTESIAN_POINT ( 'NONE',  ( -5.330712181944245322E-15, -29.10791014587222847, -8.745943564552380423 ) ) ;
#3385 = CARTESIAN_POINT ( 'NONE',  ( 2.864755990943265829, 21.99680007765647716, 2.011557305968487697 ) ) ;
#3386 = ADVANCED_FACE ( 'NONE', ( #17815 ), #14558, .F. ) ;
#3387 = VECTOR ( 'NONE', #2552, 1000.000000000000000 ) ;
#3388 = DIRECTION ( 'NONE',  ( -0.000000000000000000, -1.000000000000000000, -0.000000000000000000 ) ) ;
#3389 = DIRECTION ( 'NONE',  ( 0.000000000000000000, 0.000000000000000000, -1.000000000000000000 ) ) ;
#3390 = CARTESIAN_POINT ( 'NONE',  ( 4.730628863548789710E-15, -21.49956243961515767, -14.96605739982588368 ) ) ;
#3391 = CARTESIAN_POINT ( 'NONE',  ( -1.999999999999996225, -21.44442734547602569, -12.38381296236458162 ) ) ;
#3392 = CARTESIAN_POINT ( 'NONE',  ( -4.243569643749998122, -22.39878681574689878, -11.97879278857096885 ) ) ;
#3393 = CARTESIAN_POINT ( 'NONE',  ( 3.579096709490575479E-14, -23.06325612239561451, -1.682476010276811040 ) ) ;
#3394 = DIRECTION ( 'NONE',  ( -0.000000000000000000, -1.000000000000000000, -0.000000000000000000 ) ) ;
#3395 = CARTESIAN_POINT ( 'NONE',  ( 8.000000000000005329, 31.99999999999999289, 2.499999999999997780 ) ) ;
#3396 = CARTESIAN_POINT ( 'NONE',  ( -4.243569643750000786, -23.09367458642858040, -8.699705261538101198 ) ) ;
#3397 = CARTESIAN_POINT ( 'NONE',  ( 0.000000000000000000, 20.99999999999999289, 2.500000000000000000 ) ) ;
#3398 = CARTESIAN_POINT ( 'NONE',  ( 0.000000000000000000, 5.977523610840987267, 32.81826849749789687 ) ) ;
#3399 = CARTESIAN_POINT ( 'NONE',  ( -1.497042530366477164, 30.12180007765648426, 2.161531897785062384 ) ) ;
#3400 = EDGE_CURVE ( 'NONE', #3107, #13234, #13337, .T. ) ;
#3401 = ORIENTED_EDGE ( 'NONE', *, *, #2931, .F. ) ;
#3402 = CARTESIAN_POINT ( 'NONE',  ( 3.500000000000000444, 31.74680007765647716, -0.05647727720536935281 ) ) ;
#3403 = CARTESIAN_POINT ( 'NONE',  ( 20.00000000000000000, 3.309499999999999886, 0.000000000000000000 ) ) ;
#3404 = FILL_AREA_STYLE ('',( #10149 ) ) ;
#3405 = CARTESIAN_POINT ( 'NONE',  ( 3.999999999999996447, -27.12020499893502645, -10.42386873716718121 ) ) ;
#3406 = DIRECTION ( 'NONE',  ( -0.000000000000000000, -1.000000000000000000, -0.000000000000000000 ) ) ;
#3407 = CARTESIAN_POINT ( 'NONE',  ( 3.500000000000000444, 15.75319992234354416, 0.05647727720529520379 ) ) ;
#3408 = VERTEX_POINT ( 'NONE', #6099 ) ;
#3409 = CARTESIAN_POINT ( 'NONE',  ( -4.243569643750000786, -23.38404765733129764, -9.114400983959404456 ) ) ;
#3410 = CARTESIAN_POINT ( 'NONE',  ( -4.499999999999999112, 37.99680007765646650, 0.05647727720537927543 ) ) ;
#3411 = ORIENTED_EDGE ( 'NONE', *, *, #12016, .T. ) ;
#3412 = CYLINDRICAL_SURFACE ( 'NONE', #16128, 2.000000000000001776 ) ;
#3413 = PLANE ( 'NONE',  #273 ) ;
#3414 = CARTESIAN_POINT ( 'NONE',  ( 4.243569643750003451, -23.29141514481821318, -13.25359815749571268 ) ) ;
#3415 = DIRECTION ( 'NONE',  ( -1.000000000000000000, 0.000000000000000000, 0.000000000000000000 ) ) ;
#3416 = CARTESIAN_POINT ( 'NONE',  ( 7.706178721746812954, -10.26817993880334257, 8.683600939131450147 ) ) ;
#3417 = ADVANCED_BREP_SHAPE_REPRESENTATION ( '', ( #14274, #16940 ), #1250 ) ;
#3418 = DIRECTION ( 'NONE',  ( 0.000000000000000000, 0.000000000000000000, -1.000000000000000000 ) ) ;
#3419 =( BOUNDED_CURVE ( )  B_SPLINE_CURVE ( 2, ( #7711, #13640, #9104, #4846, #7614, #1990, #13462, #10860, #15050 ),
 .UNSPECIFIED., .F., .T. ) 
 B_SPLINE_CURVE_WITH_KNOTS ( ( 3, 2, 2, 2, 3 ),
 ( 0.2155172413793103592, 0.2183908045977011603, 0.2241379310344827624, 0.2298850574712643646, 0.2327586206896551657 ),
 .UNSPECIFIED. ) 
 CURVE ( )  GEOMETRIC_REPRESENTATION_ITEM ( )  RATIONAL_B_SPLINE_CURVE ( ( 0.9330127018922192983, 0.9330127018922196314, 1.000000000000000000, 0.8660254037844387076, 1.000000000000000000, 0.8660254037844387076, 1.000000000000000000, 0.9330127018922194093, 0.9330127018922194093 ) ) 
 REPRESENTATION_ITEM ( '' )  );
#3420 = CARTESIAN_POINT ( 'NONE',  ( 4.243569643749996345, -28.86471381881699116, -12.67011332646282895 ) ) ;
#3421 = VERTEX_POINT ( 'NONE', #4810 ) ;
#3422 = DIRECTION ( 'NONE',  ( -0.000000000000000000, -1.000000000000000000, -0.000000000000000000 ) ) ;
#3423 = CARTESIAN_POINT ( 'NONE',  ( 4.713407268011036227E-15, -19.03593212693084524, -10.95728427029060725 ) ) ;
#3424 = CARTESIAN_POINT ( 'NONE',  ( -1.734723475976807094E-15, 20.99999999999999289, -2.500000000000000000 ) ) ;
#3425 = EDGE_LOOP ( 'NONE', ( #17917, #15285, #1937, #1125, #8932 ) ) ;
#3426 = ORIENTED_EDGE ( 'NONE', *, *, #11240, .T. ) ;
#3427 = DIRECTION ( 'NONE',  ( 3.469446951953612217E-16, -0.000000000000000000, 1.000000000000000000 ) ) ;
#3428 = PLANE ( 'NONE',  #14596 ) ;
#3429 = CARTESIAN_POINT ( 'NONE',  ( -1.336863392178569088, 27.50319992234354771, -4.297206761780648421 ) ) ;
#3430 = CARTESIAN_POINT ( 'NONE',  ( -1.027846397803611866, 32.50319992234354771, -3.346150245485499219 ) ) ;
#3431 = CARTESIAN_POINT ( 'NONE',  ( -2.481649420246391902, 17.12819992234354416, -0.8687765177875723666 ) ) ;
#3432 = ORIENTED_EDGE ( 'NONE', *, *, #2173, .F. ) ;
#3433 = CARTESIAN_POINT ( 'NONE',  ( -0.05938372350918959958, 38.87819992234354771, 4.731580009072201776 ) ) ;
#3434 = CARTESIAN_POINT ( 'NONE',  ( 1.999999999999994449, -24.92574931576309538, -5.276702273821968880 ) ) ;
#3435 = ORIENTED_EDGE ( 'NONE', *, *, #15188, .T. ) ;
#3436 = ADVANCED_FACE ( 'NONE', ( #9068 ), #17445, .F. ) ;
#3437 = DIRECTION ( 'NONE',  ( 0.000000000000000000, 0.8191520442889952403, -0.5735764363510413855 ) ) ;
#3438 = EDGE_CURVE ( 'NONE', #7494, #16052, #12801, .T. ) ;
#3439 = CARTESIAN_POINT ( 'NONE',  ( 2.000000000000004441, -22.51988316363423337, -13.91972304540644245 ) ) ;
#3440 = EDGE_CURVE ( 'NONE', #5643, #9512, #12120, .T. ) ;
#3441 = CARTESIAN_POINT ( 'NONE',  ( -2.121784821875005722, -24.25430638244851167, -3.950024080123402559 ) ) ;
#3442 = CARTESIAN_POINT ( 'NONE',  ( -4.243569643750000786, -23.64215705368926379, -9.483019403889452192 ) ) ;
#3443 = EDGE_CURVE ( 'NONE', #1302, #13916, #4896, .T. ) ;
#3444 = DIRECTION ( 'NONE',  ( -1.000000000000000000, -0.000000000000000000, -0.000000000000000000 ) ) ;
#3445 = ORIENTED_EDGE ( 'NONE', *, *, #1176, .F. ) ;
#3446 = CIRCLE ( 'NONE', #1379, 2.000000000000001776 ) ;
#3447 = CARTESIAN_POINT ( 'NONE',  ( 4.772237607920560620, -11.09252097142802640, 18.58920227068357178 ) ) ;
#3448 = DIRECTION ( 'NONE',  ( -0.000000000000000000, 0.5000000000000002220, -0.8660254037844384856 ) ) ;
#3449 = VERTEX_POINT ( 'NONE', #648 ) ;
#3450 = CARTESIAN_POINT ( 'NONE',  ( 2.115076519116426024, 26.12819992234354771, 3.012182706137062294 ) ) ;
#3451 = CARTESIAN_POINT ( 'NONE',  ( -1.055605843668875110, 15.00000000000000888, -3.337496964141338562 ) ) ;
#3452 = CARTESIAN_POINT ( 'NONE',  ( -2.121784821874996396, -18.06140184503912494, -7.920110144002082464 ) ) ;
#3453 = CARTESIAN_POINT ( 'NONE',  ( 0.05938372350926800214, 22.37180007765647716, 2.628655560595669183 ) ) ;
#3454 = EDGE_CURVE ( 'NONE', #15329, #1285, #6590, .T. ) ;
#3455 = CARTESIAN_POINT ( 'NONE',  ( 2.733110507866328920, 18.62819992234354771, 3.862833514489095510 ) ) ;
#3456 = CARTESIAN_POINT ( 'NONE',  ( 1.071796769724485232, -23.11625677147122104, -1.758168781610173204 ) ) ;
#3457 = CARTESIAN_POINT ( 'NONE',  ( 2.000000000000004441, -23.55232074906610507, -15.39419672512663340 ) ) ;
#3458 = CARTESIAN_POINT ( 'NONE',  ( 4.243569643749996345, -23.21857077348643017, -4.606585390493037835 ) ) ;
#3459 = VECTOR ( 'NONE', #8843, 1000.000000000000000 ) ;
#3460 = CARTESIAN_POINT ( 'NONE',  ( -8.500000000000005329, 13.00000000000000178, -22.64999999999999147 ) ) ;
#3461 = CARTESIAN_POINT ( 'NONE',  ( -14.99999999999999645, 10.00000000000000000, 30.00000000000000000 ) ) ;
#3462 = DIRECTION ( 'NONE',  ( 0.000000000000000000, 1.000000000000000000, 0.000000000000000000 ) ) ;
#3463 = CARTESIAN_POINT ( 'NONE',  ( 4.000000000000000000, -3.518949890710769246, 4.119968255444916849E-15 ) ) ;
#3464 = ORIENTED_EDGE ( 'NONE', *, *, #16720, .T. ) ;
#3465 = EDGE_LOOP ( 'NONE', ( #16428, #11013, #9702, #13555 ) ) ;
#3466 = APPLICATION_CONTEXT ( 'automotive_design' ) ;
#3467 = VECTOR ( 'NONE', #5457, 1000.000000000000000 ) ;
#3468 = DIRECTION ( 'NONE',  ( -3.469446951953612217E-16, 0.000000000000000000, -1.000000000000000000 ) ) ;
#3469 = DIRECTION ( 'NONE',  ( -1.000000000000000000, -0.000000000000000000, -0.000000000000000000 ) ) ;
#3470 = VERTEX_POINT ( 'NONE', #17638 ) ;
#3471 = CARTESIAN_POINT ( 'NONE',  ( -2.518350579753611207, 31.87819992234354416, 0.7558219633769609480 ) ) ;
#3472 = AXIS2_PLACEMENT_3D ( 'NONE', #4111, #5323, #18146 ) ;
#3473 = CARTESIAN_POINT ( 'NONE',  ( 4.243569643750000786, -25.28760445547132107, -11.83296183094350340 ) ) ;
#3474 = CARTESIAN_POINT ( 'NONE',  ( 1.027846397803542144, 21.24680007765647716, -3.346150245485522312 ) ) ;
#3475 = CARTESIAN_POINT ( 'NONE',  ( 9.999999999999998224, 34.19999999999999574, -2.500000000000001776 ) ) ;
#3476 = CARTESIAN_POINT ( 'NONE',  ( 2.220605816132281252, -15.34963770581821763, -10.14223552587152888 ) ) ;
#3477 = CARTESIAN_POINT ( 'NONE',  ( -5.330712181944245322E-15, -29.91450200949088156, -9.897876126833780930 ) ) ;
#3478 = TOROIDAL_SURFACE ( 'NONE', #5832, 9.000000000000001776, 0.9999999999999991118 ) ;
#3479 = CARTESIAN_POINT ( 'NONE',  ( 2.121784821875004390, -21.45984223041904926, -12.77358600641437469 ) ) ;
#3480 = CARTESIAN_POINT ( 'NONE',  ( 3.608366422512736094, -25.49736372916365212, -15.63892331459559593 ) ) ;
#3481 = FACE_OUTER_BOUND ( 'NONE', #7497, .T. ) ;
#3482 = CARTESIAN_POINT ( 'NONE',  ( -2.121784821875005722, -26.57729094967022831, -7.267589859493831739 ) ) ;
#3483 = ORIENTED_EDGE ( 'NONE', *, *, #3497, .T. ) ;
#3484 = CARTESIAN_POINT ( 'NONE',  ( 1.533898589781675205E-14, -27.45111586048108521, -7.948989149087622330 ) ) ;
#3485 = CARTESIAN_POINT ( 'NONE',  ( -3.500000000000000444, 40.00000000000000711, 3.664603343001004987E-14 ) ) ;
#3486 = CARTESIAN_POINT ( 'NONE',  ( 0.05938372350926800214, 27.37180007765647716, 2.628655560595669183 ) ) ;
#3487 = ORIENTED_EDGE ( 'NONE', *, *, #10565, .F. ) ;
#3488 = CARTESIAN_POINT ( 'NONE',  ( 2.115076519116362963, 28.87180007765647716, -3.012182706137107591 ) ) ;
#3489 = CARTESIAN_POINT ( 'NONE',  ( -1.071796769724486564, -27.01095111827842388, -7.320368749872718794 ) ) ;
#3490 = PRODUCT_CONTEXT ( 'NONE', #10071, 'mechanical' ) ;
#3491 = CIRCLE ( 'NONE', #6735, 8.000000000000001776 ) ;
#3492 = CARTESIAN_POINT ( 'NONE',  ( 4.000000000000000000, 1.759474945355387954, 3.047499999999997211 ) ) ;
#3493 = AXIS2_PLACEMENT_3D ( 'NONE', #9128, #14620, #14808 ) ;
#3494 = CARTESIAN_POINT ( 'NONE',  ( -3.500000000000000444, 22.00319992234354416, -0.05647727720529563400 ) ) ;
#3495 = ORIENTED_EDGE ( 'NONE', *, *, #8063, .T. ) ;
#3496 = CARTESIAN_POINT ( 'NONE',  ( -2.121784821874996396, -19.90043129408965328, -10.54651638600367214 ) ) ;
#3497 = EDGE_CURVE ( 'NONE', #5271, #11449, #9412, .T. ) ;
#3498 = CARTESIAN_POINT ( 'NONE',  ( -4.499999999999999112, 40.49680007765648071, 0.05647727720537927543 ) ) ;
#3499 = EDGE_LOOP ( 'NONE', ( #10498, #8414, #3226, #10524 ) ) ;
#3500 = EDGE_CURVE ( 'NONE', #10466, #15990, #15193, .T. ) ;
#3501 = CARTESIAN_POINT ( 'NONE',  ( 8.000000000000005329, 20.99999999999999289, 2.499999999999997780 ) ) ;
#3502 = CARTESIAN_POINT ( 'NONE',  ( -5.330712181944245322E-15, -29.65639261313291541, -9.529257706903733194 ) ) ;
#3503 = CARTESIAN_POINT ( 'NONE',  ( 13.80999999999999872, 2.449293598294706907E-16, -2.000000000000000444 ) ) ;
#3504 =( GEOMETRIC_REPRESENTATION_CONTEXT ( 3 ) GLOBAL_UNCERTAINTY_ASSIGNED_CONTEXT ( ( #13791 ) ) GLOBAL_UNIT_ASSIGNED_CONTEXT ( ( #15992, #17206, #413 ) ) REPRESENTATION_CONTEXT ( 'NONE', 'WORKASPACE' ) );
#3505 = CARTESIAN_POINT ( 'NONE',  ( 9.999999999999998224, 20.99999999999999289, -2.500000000000001776 ) ) ;
#3506 = ADVANCED_FACE ( 'NONE', ( #17722 ), #17580, .T. ) ;
#3508 = LINE ( 'NONE', #14547, #14137 ) ;
#3507 = TOROIDAL_SURFACE ( 'NONE', #16559, 9.000000000000001776, 0.9999999999999991118 ) ;
#3509 = CARTESIAN_POINT ( 'NONE',  ( 2.121784821875004390, -17.36235556323629936, -6.921768590024867329 ) ) ;
#3510 = VERTEX_POINT ( 'NONE', #9252 ) ;
#3511 = CARTESIAN_POINT ( 'NONE',  ( 4.000000000000000888, -23.14207009859818243, -8.768821215778363154 ) ) ;
#3512 = CARTESIAN_POINT ( 'NONE',  ( 1.999999999999994449, -26.28082364734737908, -7.211948979461484832 ) ) ;
#3513 = EDGE_LOOP ( 'NONE', ( #4686, #17563, #7440, #5711 ) ) ;
#3514 = EDGE_LOOP ( 'NONE', ( #12299, #6468, #2485, #7809 ) ) ;
#3515 = CARTESIAN_POINT ( 'NONE',  ( -1.999999999999996225, -18.60522398553836965, -8.329010343134054750 ) ) ;
#3516 = CARTESIAN_POINT ( 'NONE',  ( 8.000000000000001776, 29.79999999999999716, -2.500000000000002220 ) ) ;
#3517 = CARTESIAN_POINT ( 'NONE',  ( -3.673772985318163098, 24.25319992234354061, 2.599342558261029001 ) ) ;
#3518 = CARTESIAN_POINT ( 'NONE',  ( 1.135272562821020070, 35.25319992234354771, -3.311245368580577164 ) ) ;
#3519 = CARTESIAN_POINT ( 'NONE',  ( 0.8262555684460829442, 22.75319992234354771, -2.360188852285421302 ) ) ;
#3520 = ORIENTED_EDGE ( 'NONE', *, *, #2483, .T. ) ;
#3521 = VECTOR ( 'NONE', #12068, 1000.000000000000000 ) ;
#3522 = CARTESIAN_POINT ( 'NONE',  ( -4.499999999999999112, 15.49680007765647538, 0.05647727720537927543 ) ) ;
#3523 = TOROIDAL_SURFACE ( 'NONE', #13576, 9.000000000000001776, 0.9999999999999991118 ) ;
#3524 = CARTESIAN_POINT ( 'NONE',  ( -5.279047395330986450E-15, -26.15124313503919495, -5.013729875556656168 ) ) ;
#3525 = ORIENTED_EDGE ( 'NONE', *, *, #14847, .T. ) ;
#3526 = DIRECTION ( 'NONE',  ( 0.000000000000000000, 0.000000000000000000, -1.000000000000000000 ) ) ;
#3527 = CARTESIAN_POINT ( 'NONE',  ( -1.135272562821090014, 38.49680007765647360, -3.311245368580554072 ) ) ;
#3528 =( BOUNDED_CURVE ( )  B_SPLINE_CURVE ( 2, ( #16539, #3815, #12772, #16726, #5301, #4001, #10952, #15140, #12951 ),
 .UNSPECIFIED., .F., .T. ) 
 B_SPLINE_CURVE_WITH_KNOTS ( ( 3, 2, 2, 2, 3 ),
 ( 0.1465517241379310498, 0.1494252873563218509, 0.1551724137931034531, 0.1609195402298850552, 0.1637931034482758563 ),
 .UNSPECIFIED. ) 
 CURVE ( )  GEOMETRIC_REPRESENTATION_ITEM ( )  RATIONAL_B_SPLINE_CURVE ( ( 0.9330127018922192983, 0.9330127018922196314, 1.000000000000000000, 0.8660254037844387076, 1.000000000000000000, 0.8660254037844387076, 1.000000000000000000, 0.9330127018922194093, 0.9330127018922194093 ) ) 
 REPRESENTATION_ITEM ( '' )  );
#3529 = CARTESIAN_POINT ( 'NONE',  ( -5.577813053751546416E-15, -28.74166284227092305, -9.792081248737861898 ) ) ;
#3530 = CARTESIAN_POINT ( 'NONE',  ( -5.330712181944246111E-15, -24.20383161507082193, -1.742193585881474771 ) ) ;
#3531 = CARTESIAN_POINT ( 'NONE',  ( 2.121784821875004390, -20.97588711224786095, -12.08242646904553474 ) ) ;
#3532 = PRODUCT_DEFINITION_SHAPE ( 'NONE', 'NONE',  #13528 ) ;
#3533 = CIRCLE ( 'NONE', #8263, 2.000000000000000000 ) ;
#3534 = DIRECTION ( 'NONE',  ( 0.000000000000000000, -0.000000000000000000, -1.000000000000000000 ) ) ;
#3535 = AXIS2_PLACEMENT_3D ( 'NONE', #6208, #14946, #4627 ) ;
#3536 = ORIENTED_EDGE ( 'NONE', *, *, #1110, .T. ) ;
#3537 = CARTESIAN_POINT ( 'NONE',  ( -0.6435604995507047121, -10.54254386713301628, 22.30101802474215233 ) ) ;
#3538 = EDGE_CURVE ( 'NONE', #12774, #8670, #11313, .T. ) ;
#3539 = DIRECTION ( 'NONE',  ( 0.000000000000000000, -9.859324684083080328E-16, -1.000000000000000000 ) ) ;
#3540 = CARTESIAN_POINT ( 'NONE',  ( -5.577813053751546416E-15, -25.96698683212770931, -5.829433235496615850 ) ) ;
#3541 = ORIENTED_EDGE ( 'NONE', *, *, #6831, .T. ) ;
#3542 = CARTESIAN_POINT ( 'NONE',  ( 1.027846397803612311, 31.25319992234354416, 3.346150245485499219 ) ) ;
#3543 = CARTESIAN_POINT ( 'NONE',  ( -9.000000000000001776, 38.59999999999999432, 2.499999999999998224 ) ) ;
#3544 = CARTESIAN_POINT ( 'NONE',  ( 4.243569643750000786, -21.93218230281772918, -7.040922371852881945 ) ) ;
#3545 = CARTESIAN_POINT ( 'NONE',  ( 2.518350579753628971, 19.37180007765648071, 0.7558219633769073242 ) ) ;
#3546 = CARTESIAN_POINT ( 'NONE',  ( 1.336863392178569754, 16.25319992234354416, 4.297206761780648421 ) ) ;
#3547 = CARTESIAN_POINT ( 'NONE',  ( -4.243569643749998122, -24.23781626479742712, -14.60519903057256208 ) ) ;
#3548 = CARTESIAN_POINT ( 'NONE',  ( -2.000000000000005773, -28.84040849385894845, -10.86741497609436280 ) ) ;
#3549 = CIRCLE ( 'NONE', #885, 7.000000000000000000 ) ;
#3550 = CARTESIAN_POINT ( 'NONE',  ( -5.330712181944245322E-15, -25.26853287504744472, -3.262744568092923014 ) ) ;
#3551 = AXIS2_PLACEMENT_3D ( 'NONE', #12405, #18096, #5368 ) ;
#3552 = CARTESIAN_POINT ( 'NONE',  ( 3.500000000000000444, 16.74680007765647716, -0.05647727720536935281 ) ) ;
#3553 = DIRECTION ( 'NONE',  ( -0.000000000000000000, -1.000000000000000000, -0.000000000000000000 ) ) ;
#3554 = CIRCLE ( 'NONE', #6511, 8.000000000000001776 ) ;
#3555 = DIRECTION ( 'NONE',  ( 0.000000000000000000, 0.000000000000000000, -1.000000000000000000 ) ) ;
#3556 = VERTEX_POINT ( 'NONE', #13511 ) ;
#3557 = ORIENTED_EDGE ( 'NONE', *, *, #12833, .T. ) ;
#3558 = FACE_BOUND ( 'NONE', #12798, .T. ) ;
#3559 = EDGE_CURVE ( 'NONE', #16544, #5572, #10717, .T. ) ;
#3560 = CARTESIAN_POINT ( 'NONE',  ( 3.999999999999996447, -22.66781791105512767, -4.065200992367092425 ) ) ;
#3561 = CARTESIAN_POINT ( 'NONE',  ( 4.299564228933482956E-15, -22.57561058249592278, -14.93362036944126814 ) ) ;
#3562 = ORIENTED_EDGE ( 'NONE', *, *, #4707, .F. ) ;
#3563 = TOROIDAL_SURFACE ( 'NONE', #11843, 9.000000000000001776, 0.9999999999999991118 ) ;
#3564 = CARTESIAN_POINT ( 'NONE',  ( -2.500000000000001332, 24.50319992234354771, -0.05647727720530596601 ) ) ;
#3565 = EDGE_CURVE ( 'NONE', #10757, #18352, #7019, .T. ) ;
#3566 = CARTESIAN_POINT ( 'NONE',  ( -4.243569643749997233, -24.20555259025267603, -14.55912172808130656 ) ) ;
#3567 = CARTESIAN_POINT ( 'NONE',  ( -2.864755990943265829, 23.24680007765647716, -2.011557305968488141 ) ) ;
#3568 = CARTESIAN_POINT ( 'NONE',  ( -9.000000000000001776, 43.00000000000000000, 2.499999999999998224 ) ) ;
#3569 = CARTESIAN_POINT ( 'NONE',  ( 4.730628863548789710E-15, -22.01578123233109707, -15.70329423968597915 ) ) ;
#3570 = TOROIDAL_SURFACE ( 'NONE', #13641, 9.000000000000001776, 0.9999999999999991118 ) ;
#3571 = AXIS2_PLACEMENT_3D ( 'NONE', #7197, #16302, #4600 ) ;
#3572 = DIRECTION ( 'NONE',  ( 0.000000000000000000, 0.000000000000000000, 1.000000000000000000 ) ) ;
#3573 = DIRECTION ( 'NONE',  ( 0.000000000000000000, 0.000000000000000000, 1.000000000000000000 ) ) ;
#3574 = CARTESIAN_POINT ( 'NONE',  ( 4.243569643750003451, -20.93616690305174544, -9.889955075634029313 ) ) ;
#3575 = CARTESIAN_POINT ( 'NONE',  ( 1.533898589781675205E-14, -27.19300646412311551, -7.580370729157575482 ) ) ;
#3576 = CARTESIAN_POINT ( 'NONE',  ( -8.500000000000005329, 10.00000000000000000, 20.49999999999999645 ) ) ;
#3577 = CARTESIAN_POINT ( 'NONE',  ( -2.481649420246374138, 27.87180007765648426, 0.8687765177876256573 ) ) ;
#3578 = VERTEX_POINT ( 'NONE', #13788 ) ;
#3579 = CARTESIAN_POINT ( 'NONE',  ( 1.027846397803542144, 26.24680007765648071, -3.346150245485522312 ) ) ;
#3580 = CARTESIAN_POINT ( 'NONE',  ( 0.000000000000000000, 5.000000000000000000, 0.000000000000000000 ) ) ;
#3581 = APPLICATION_PROTOCOL_DEFINITION ( 'draft international standard', 'automotive_design', 1998, #6307 ) ;
#3582 = AXIS2_PLACEMENT_3D ( 'NONE', #3866, #7761, #6284 ) ;
#3583 = FACE_OUTER_BOUND ( 'NONE', #8947, .T. ) ;
#3584 = VERTEX_POINT ( 'NONE', #5443 ) ;
#3585 = CARTESIAN_POINT ( 'NONE',  ( -2.121784821875005722, -25.57711703878310061, -5.839193482264897206 ) ) ;
#3586 = CARTESIAN_POINT ( 'NONE',  ( 2.115076519116362963, 16.37180007765647716, -3.012182706137107147 ) ) ;
#3587 = ORIENTED_EDGE ( 'NONE', *, *, #11512, .T. ) ;
#3588 = DIRECTION ( 'NONE',  ( -0.000000000000000000, -1.000000000000000000, -0.000000000000000000 ) ) ;
#3589 = DIRECTION ( 'NONE',  ( 0.000000000000000000, 0.000000000000000000, -1.000000000000000000 ) ) ;
#3590 = CARTESIAN_POINT ( 'NONE',  ( -3.250871920745033616, -25.09854970161199716, -15.79815562995958977 ) ) ;
#3591 =( GEOMETRIC_REPRESENTATION_CONTEXT ( 3 ) GLOBAL_UNCERTAINTY_ASSIGNED_CONTEXT ( ( #8257 ) ) GLOBAL_UNIT_ASSIGNED_CONTEXT ( ( #8924, #6342, #16364 ) ) REPRESENTATION_CONTEXT ( 'NONE', 'WORKASPACE' ) );
#3592 = CARTESIAN_POINT ( 'NONE',  ( 9.000000000000005329, -10.00000000000000178, 15.14468620625654616 ) ) ;
#3593 = CARTESIAN_POINT ( 'NONE',  ( 1.533898589781675205E-14, -27.96733465319702105, -8.686225988947720467 ) ) ;
#3594 = CARTESIAN_POINT ( 'NONE',  ( 4.243569643750000786, -27.09437022997710187, -14.41329077045383578 ) ) ;
#3595 = ORIENTED_EDGE ( 'NONE', *, *, #17528, .T. ) ;
#3596 = CARTESIAN_POINT ( 'NONE',  ( 4.000000000000003553, -21.22881036912508179, -10.06272105382992521 ) ) ;
#3597 = CARTESIAN_POINT ( 'NONE',  ( 4.713407268011036227E-15, -18.77782273057287910, -10.58866585036055596 ) ) ;
#3598 = ORIENTED_EDGE ( 'NONE', *, *, #4237, .T. ) ;
#3599 = ORIENTED_EDGE ( 'NONE', *, *, #13575, .F. ) ;
#3600 = DIRECTION ( 'NONE',  ( 0.000000000000000000, 0.000000000000000000, -1.000000000000000000 ) ) ;
#3601 = EDGE_CURVE ( 'NONE', #9347, #10311, #5169, .T. ) ;
#3602 = CARTESIAN_POINT ( 'NONE',  ( 4.481649420246397675, 33.37819992234354771, 1.518615910253363177 ) ) ;
#3603 = CIRCLE ( 'NONE', #13068, 0.9999999999999991118 ) ;
#3604 = CARTESIAN_POINT ( 'NONE',  ( 2.115076519116425580, 33.62819992234354061, 3.012182706137062294 ) ) ;
#3605 = EDGE_CURVE ( 'NONE', #1028, #10466, #8630, .T. ) ;
#3606 = CARTESIAN_POINT ( 'NONE',  ( -2.055738996568281518, 19.25319992234354416, 1.423772053676066962 ) ) ;
#3607 = ORIENTED_EDGE ( 'NONE', *, *, #6701, .T. ) ;
#3608 = COLOUR_RGB ( '',0.8941176470588234615, 0.8941176470588234615, 0.8941176470588234615 ) ;
#3609 = CARTESIAN_POINT ( 'NONE',  ( 4.518350579753633411, 16.87180007765647716, 1.405661355842698468 ) ) ;
#3610 = CARTESIAN_POINT ( 'NONE',  ( -4.000000000000004441, -23.27007316922370350, -4.925310638870541879 ) ) ;
#3611 = ORIENTED_EDGE ( 'NONE', *, *, #13294, .F. ) ;
#3612 = CARTESIAN_POINT ( 'NONE',  ( -8.999999999999996447, -10.00000000000000000, 15.14468620625656925 ) ) ;
#3613 = DIRECTION ( 'NONE',  ( 0.000000000000000000, -0.4999999999999992784, 0.8660254037844389297 ) ) ;
#3614 = CARTESIAN_POINT ( 'NONE',  ( 2.000000000000004441, -20.97122678548641872, -11.70801252582615604 ) ) ;
#3615 = AXIS2_PLACEMENT_3D ( 'NONE', #16001, #8933, #13198 ) ;
#3616 = CARTESIAN_POINT ( 'NONE',  ( -4.243569643750004339, -21.72368718624651507, -2.471670375064849434 ) ) ;
#3617 =( GEOMETRIC_REPRESENTATION_CONTEXT ( 3 ) GLOBAL_UNCERTAINTY_ASSIGNED_CONTEXT ( ( #16777 ) ) GLOBAL_UNIT_ASSIGNED_CONTEXT ( ( #5096, #13720, #1031 ) ) REPRESENTATION_CONTEXT ( 'NONE', 'WORKASPACE' ) );
#3618 = CARTESIAN_POINT ( 'NONE',  ( 4.243569643750003451, -22.00086816302836823, -11.41050605784547578 ) ) ;
#3619 = PRODUCT_DEFINITION_FORMATION_WITH_SPECIFIED_SOURCE ( 'ANY', '', #4859, .NOT_KNOWN. ) ;
#3620 = CARTESIAN_POINT ( 'NONE',  ( -3.500000000000000444, 39.50319992234354061, -0.05647727720529600870 ) ) ;
#3621 = ORIENTED_EDGE ( 'NONE', *, *, #9034, .F. ) ;
#3622 = ADVANCED_FACE ( 'NONE', ( #6739 ), #2751, .T. ) ;
#3623 = CARTESIAN_POINT ( 'NONE',  ( 1.287074048710447283, -10.56983422227372671, 22.11683441173062192 ) ) ;
#3624 = DIRECTION ( 'NONE',  ( -0.000000000000000000, 1.000000000000000000, -0.000000000000000000 ) ) ;
#3625 = DIRECTION ( 'NONE',  ( -0.000000000000000000, 1.000000000000000000, -0.000000000000000000 ) ) ;
#3626 = CARTESIAN_POINT ( 'NONE',  ( -4.000000000000000888, -22.75490600406122255, -8.215893585883295103 ) ) ;
#3627 = ORIENTED_EDGE ( 'NONE', *, *, #17741, .T. ) ;
#3628 = CARTESIAN_POINT ( 'NONE',  ( -1.027846397803611866, 27.50319992234354771, -3.346150245485499219 ) ) ;
#3629 = CARTESIAN_POINT ( 'NONE',  ( -8.500000000000005329, 10.00000000000000000, -22.50000000000000000 ) ) ;
#3630 = EDGE_CURVE ( 'NONE', #2315, #15771, #6817, .T. ) ;
#3631 = CARTESIAN_POINT ( 'NONE',  ( 2.121784821875004390, -17.58820128504952152, -7.244309707463659542 ) ) ;
#3632 = CARTESIAN_POINT ( 'NONE',  ( -0.8262555684461330152, 25.99680007765648071, -2.360188852285403982 ) ) ;
#3633 = VECTOR ( 'NONE', #7832, 999.9999999999998863 ) ;
#3634 = CARTESIAN_POINT ( 'NONE',  ( -3.500000000000000444, 39.50319992234354771, -0.05647727720529563400 ) ) ;
#3635 = AXIS2_PLACEMENT_3D ( 'NONE', #13994, #9900, #5554 ) ;
#3636 = CARTESIAN_POINT ( 'NONE',  ( 1.999999999999994449, -28.79739026113263023, -10.80597857277268403 ) ) ;
#3637 =( BOUNDED_CURVE ( )  B_SPLINE_CURVE ( 2, ( #1951, #5233, #16566, #6534, #12364, #16038, #3847, #13763, #17539 ),
 .UNSPECIFIED., .F., .T. ) 
 B_SPLINE_CURVE_WITH_KNOTS ( ( 3, 2, 2, 2, 3 ),
 ( 0.2327586206896551657, 0.2356321839080459668, 0.2413793103448275967, 0.2471264367816091989, 0.2500000000000000000 ),
 .UNSPECIFIED. ) 
 CURVE ( )  GEOMETRIC_REPRESENTATION_ITEM ( )  RATIONAL_B_SPLINE_CURVE ( ( 0.9330127018922194093, 0.9330127018922194093, 1.000000000000000000, 0.8660254037844387076, 1.000000000000000000, 0.8660254037844387076, 1.000000000000000000, 0.9330127018922197424, 0.9330127018922194093 ) ) 
 REPRESENTATION_ITEM ( '' )  );
#3638 = ORIENTED_EDGE ( 'NONE', *, *, #16368, .F. ) ;
#3639 = CARTESIAN_POINT ( 'NONE',  ( -2.121784821874996396, -18.86799370865777803, -9.072042706283481195 ) ) ;
#3640 = CARTESIAN_POINT ( 'NONE',  ( -1.135272562821090014, 15.99680007765647716, -3.311245368580554072 ) ) ;
#3641 = CARTESIAN_POINT ( 'NONE',  ( -15.00000000000000178, 13.00000000000000178, 24.99999999999999645 ) ) ;
#3642 = AXIS2_PLACEMENT_3D ( 'NONE', #16523, #10485, #16338 ) ;
#3643 = LINE ( 'NONE', #9015, #16917 ) ;
#3644 = AXIS2_PLACEMENT_3D ( 'NONE', #12887, #14108, #193 ) ;
#3645 = EDGE_LOOP ( 'NONE', ( #6369, #5806 ) ) ;
#3646 = ORIENTED_EDGE ( 'NONE', *, *, #18354, .F. ) ;
#3647 = CYLINDRICAL_SURFACE ( 'NONE', #608, 0.9999999999999991118 ) ;
#3648 = CARTESIAN_POINT ( 'NONE',  ( 7.503318896749359368, -12.79558280299057316, 6.421203217138808483 ) ) ;
#3649 = VERTEX_POINT ( 'NONE', #5354 ) ;
#3650 = CARTESIAN_POINT ( 'NONE',  ( 2.500000000000001332, 25.75319992234354771, 0.05647727720530566764 ) ) ;
#3651 = CARTESIAN_POINT ( 'NONE',  ( -2.121784821874996396, -23.22358977219849407, -15.29247854260303718 ) ) ;
#3652 = CARTESIAN_POINT ( 'NONE',  ( -3.500000000000000444, 25.49680007765647716, 0.05647727720536892260 ) ) ;
#3653 = DIRECTION ( 'NONE',  ( -0.000000000000000000, -0.5735764363510414965, -0.8191520442889950182 ) ) ;
#3654 = CARTESIAN_POINT ( 'NONE',  ( 2.526502195916454863, -15.31622431267016360, -9.916727303591175158 ) ) ;
#3655 = CIRCLE ( 'NONE', #9860, 0.9999999999999991118 ) ;
#3656 = VECTOR ( 'NONE', #13907, 1000.000000000000000 ) ;
#3657 = CARTESIAN_POINT ( 'NONE',  ( -2.121784821875005722, -27.90010160600482081, -9.156759261635325942 ) ) ;
#3658 = EDGE_CURVE ( 'NONE', #8888, #10898, #12607, .T. ) ;
#3659 = EDGE_CURVE ( 'NONE', #5080, #3510, #3737, .T. ) ;
#3660 =( BOUNDED_CURVE ( )  B_SPLINE_CURVE ( 3, ( #3357, #14486, #9088, #479 ),
 .UNSPECIFIED., .F., .F. ) 
 B_SPLINE_CURVE_WITH_KNOTS ( ( 4, 4 ),
 ( 4.712388980384689674, 6.283185307179585344 ),
 .UNSPECIFIED. ) 
 CURVE ( )  GEOMETRIC_REPRESENTATION_ITEM ( )  RATIONAL_B_SPLINE_CURVE ( ( 1.000000000000000000, 0.8047378541243649375, 0.8047378541243649375, 1.000000000000000000 ) ) 
 REPRESENTATION_ITEM ( '' )  );
#3661 = CARTESIAN_POINT ( 'NONE',  ( 3.798794474141382604, -25.80746198062961838, -15.42752687081247132 ) ) ;
#3662 = CARTESIAN_POINT ( 'NONE',  ( 2.829195390882805583, 19.62180007765647716, 3.793023760679204770 ) ) ;
#3663 = EDGE_CURVE ( 'NONE', #1446, #5758, #15286, .T. ) ;
#3664 = CARTESIAN_POINT ( 'NONE',  ( -1.999999999999996225, -23.50930251633977264, -15.33276032180496173 ) ) ;
#3665 = FACE_BOUND ( 'NONE', #3976, .T. ) ;
#3666 = CARTESIAN_POINT ( 'NONE',  ( 4.730628863548789710E-15, -19.14431419784869348, -11.60241431796419853 ) ) ;
#3667 = VERTEX_POINT ( 'NONE', #16775 ) ;
#3668 = FACE_OUTER_BOUND ( 'NONE', #14133, .T. ) ;
#3669 = AXIS2_PLACEMENT_3D ( 'NONE', #3568, #10221, #4576 ) ;
#3670 = ADVANCED_FACE ( 'NONE', ( #4044 ), #3928, .T. ) ;
#3671 = CARTESIAN_POINT ( 'NONE',  ( 2.055738996568313048, 29.49680007765648426, 1.423772053676023441 ) ) ;
#3672 = ORIENTED_EDGE ( 'NONE', *, *, #7203, .T. ) ;
#3673 = CARTESIAN_POINT ( 'NONE',  ( -2.211161402132901799, 33.37180007765648071, -2.942372952327172886 ) ) ;
#3674 = DIRECTION ( 'NONE',  ( -0.000000000000000000, 1.000000000000000000, -0.000000000000000000 ) ) ;
#3675 = SHAPE_DEFINITION_REPRESENTATION ( #2061, #5199 ) ;
#3676 = DIRECTION ( 'NONE',  ( 1.000000000000000000, 0.000000000000000000, 1.224646799147353207E-16 ) ) ;
#3677 = ORIENTED_EDGE ( 'NONE', *, *, #13039, .F. ) ;
#3678 = CARTESIAN_POINT ( 'NONE',  ( 4.730628863548789710E-15, -18.91846847603547133, -11.27987320052540809 ) ) ;
#3679 = CARTESIAN_POINT ( 'NONE',  ( -1.135272562821090014, 23.49680007765647716, -3.311245368580554072 ) ) ;
#3680 = ORIENTED_EDGE ( 'NONE', *, *, #7961, .F. ) ;
#3681 = DIRECTION ( 'NONE',  ( 0.000000000000000000, 0.000000000000000000, 1.000000000000000000 ) ) ;
#3682 = CARTESIAN_POINT ( 'NONE',  ( -8.500000000000005329, 15.00000000000000178, -20.49999999999999645 ) ) ;
#3683 = CARTESIAN_POINT ( 'NONE',  ( -2.714947574412843956, -24.61702768235999272, -16.14861449798980075 ) ) ;
#3684 = DIRECTION ( 'NONE',  ( 0.000000000000000000, 0.000000000000000000, -1.000000000000000000 ) ) ;
#3685 = CARTESIAN_POINT ( 'NONE',  ( 1.071796769724485454, -21.29659030142491005, -13.10699010444694679 ) ) ;
#3686 = CARTESIAN_POINT ( 'NONE',  ( 4.243569643749996345, -21.92802379169658877, -2.763493290842798267 ) ) ;
#3687 = ORIENTED_EDGE ( 'NONE', *, *, #18287, .F. ) ;
#3688 = CARTESIAN_POINT ( 'NONE',  ( 3.999999999999993339, 7.428752623566170548E-15, 30.00000000000000000 ) ) ;
#3689 = CARTESIAN_POINT ( 'NONE',  ( 4.713407268011036227E-15, -19.55215091964678820, -11.69452111015069917 ) ) ;
#3690 = CARTESIAN_POINT ( 'NONE',  ( 2.864755990943265829, 34.49680007765648071, 2.011557305968487697 ) ) ;
#3691 = ORIENTED_EDGE ( 'NONE', *, *, #10633, .F. ) ;
#3692 = ORIENTED_EDGE ( 'NONE', *, *, #3328, .F. ) ;
#3693 = CARTESIAN_POINT ( 'NONE',  ( 4.000000000000000888, -26.23938285489380462, -13.19224225493893599 ) ) ;
#3694 = CARTESIAN_POINT ( 'NONE',  ( -3.673772985318163098, 36.75319992234353350, 2.599342558261029001 ) ) ;
#3695 = CARTESIAN_POINT ( 'NONE',  ( 2.864755990943222308, 33.00319992234354771, -2.011557305968548093 ) ) ;
#3696 = CARTESIAN_POINT ( 'NONE',  ( -1.989345975306457071, 27.25319992234354771, -1.515154207786300944 ) ) ;
#3697 = ORIENTED_EDGE ( 'NONE', *, *, #1178, .T. ) ;
#3698 = CARTESIAN_POINT ( 'NONE',  ( 3.607379964056306676, 23.99680007765647716, -2.690724712371305838 ) ) ;
#3699 = CARTESIAN_POINT ( 'NONE',  ( -4.000000000000004441, -22.23763558379183181, -3.450836959150351380 ) ) ;
#3700 = VERTEX_POINT ( 'NONE', #18353 ) ;
#3701 = CARTESIAN_POINT ( 'NONE',  ( 9.000000000000005329, 40.79999999999999716, 2.499999999999997335 ) ) ;
#3702 = CARTESIAN_POINT ( 'NONE',  ( -2.211161402132902243, 35.87180007765648782, -2.942372952327172886 ) ) ;
#3703 = CARTESIAN_POINT ( 'NONE',  ( -1.734723475976807094E-15, 34.19999999999999574, -12.50000000000000000 ) ) ;
#3704 = CARTESIAN_POINT ( 'NONE',  ( 2.769793372871041548, -22.34959508723814992, -1.882086548653339797 ) ) ;
#3705 = CARTESIAN_POINT ( 'NONE',  ( 4.243569643749996345, -26.31588352978205592, -9.030006429653610667 ) ) ;
#3706 = DIRECTION ( 'NONE',  ( 0.000000000000000000, 0.000000000000000000, -1.000000000000000000 ) ) ;
#3707 = ORIENTED_EDGE ( 'NONE', *, *, #17634, .F. ) ;
#3708 = CARTESIAN_POINT ( 'NONE',  ( -4.000000000000004441, -21.72141679107589596, -2.713600119290256352 ) ) ;
#3709 = DIRECTION ( 'NONE',  ( 0.000000000000000000, -0.000000000000000000, 1.000000000000000000 ) ) ;
#3710 = CARTESIAN_POINT ( 'NONE',  ( -1.999999999999996225, -19.89577096732821104, -10.17210244278429343 ) ) ;
#3711 = CARTESIAN_POINT ( 'NONE',  ( 4.243569643749996345, -28.89697749336173871, -12.71619062895408803 ) ) ;
#3712 = ORIENTED_EDGE ( 'NONE', *, *, #14005, .T. ) ;
#3713 = CARTESIAN_POINT ( 'NONE',  ( -1.135272562821019626, 39.00319992234354061, 3.311245368580577164 ) ) ;
#3714 = PLANE ( 'NONE',  #3642 ) ;
#3715 = CARTESIAN_POINT ( 'NONE',  ( 4.243569643749996345, -21.89576011715183768, -2.717415988351541856 ) ) ;
#3716 = CARTESIAN_POINT ( 'NONE',  ( -2.500000000000001332, 30.49680007765648071, 0.05647727720535858364 ) ) ;
#3717 = CARTESIAN_POINT ( 'NONE',  ( -1.336863392178569088, 15.00319992234354594, -4.297206761780648421 ) ) ;
#3718 = CARTESIAN_POINT ( 'NONE',  ( -4.000000000000004441, -26.62549532187730250, -9.717350097961160671 ) ) ;
#3719 = VERTEX_POINT ( 'NONE', #16867 ) ;
#3720 = AXIS2_PLACEMENT_3D ( 'NONE', #16763, #2487, #3681 ) ;
#3721 = CARTESIAN_POINT ( 'NONE',  ( 2.121784821875004390, -17.62046495959427261, -7.290387009954915953 ) ) ;
#3722 = CARTESIAN_POINT ( 'NONE',  ( -2.829195390882805139, 35.87180007765647360, -3.793023760679206102 ) ) ;
#3723 = EDGE_CURVE ( 'NONE', #11211, #5374, #5399, .T. ) ;
#3724 = TOROIDAL_SURFACE ( 'NONE', #2842, 9.000000000000001776, 0.9999999999999991118 ) ;
#3725 = FACE_OUTER_BOUND ( 'NONE', #17989, .T. ) ;
#3726 = CARTESIAN_POINT ( 'NONE',  ( 0.000000000000000000, 3.000000000000000000, 0.000000000000000000 ) ) ;
#3727 = DIRECTION ( 'NONE',  ( -0.000000000000000000, 1.000000000000000000, -0.000000000000000000 ) ) ;
#3728 = VERTEX_POINT ( 'NONE', #4143 ) ;
#3729 = ORIENTED_EDGE ( 'NONE', *, *, #18287, .T. ) ;
#3730 = CARTESIAN_POINT ( 'NONE',  ( 2.211161402132902243, 19.62180007765647360, 2.942372952327172442 ) ) ;
#3731 = FACE_OUTER_BOUND ( 'NONE', #66, .T. ) ;
#3732 = CARTESIAN_POINT ( 'NONE',  ( 4.299564228933482956E-15, -19.80093457235270549, -10.97097235620001854 ) ) ;
#3733 = ORIENTED_EDGE ( 'NONE', *, *, #10684, .F. ) ;
#3734 = CARTESIAN_POINT ( 'NONE',  ( -2.481649420246391902, 37.12819992234354771, -0.8687765177875723666 ) ) ;
#3735 = CARTESIAN_POINT ( 'NONE',  ( 4.243569643750000786, -23.73894807732350998, -9.621251311363216985 ) ) ;
#3736 = CARTESIAN_POINT ( 'NONE',  ( 2.211161402132902243, 22.12180007765648071, 2.942372952327172442 ) ) ;
#3737 =( BOUNDED_CURVE ( )  B_SPLINE_CURVE ( 2, ( #11091, #1012, #6561, #16684, #6651, #17990, #3961, #5262, #9614 ),
 .UNSPECIFIED., .F., .T. ) 
 B_SPLINE_CURVE_WITH_KNOTS ( ( 3, 2, 2, 2, 3 ),
 ( 0.8017241379310344751, 0.8045977011494253039, 0.8103448275862068506, 0.8160919540229885083, 0.8189655172413793371 ),
 .UNSPECIFIED. ) 
 CURVE ( )  GEOMETRIC_REPRESENTATION_ITEM ( )  RATIONAL_B_SPLINE_CURVE ( ( 0.9330127018922194093, 0.9330127018922194093, 1.000000000000000000, 0.8660254037844387076, 1.000000000000000000, 0.8660254037844387076, 1.000000000000000000, 0.9330127018922194093, 0.9330127018922194093 ) ) 
 REPRESENTATION_ITEM ( '' )  );
#3738 = AXIS2_PLACEMENT_3D ( 'NONE', #1055, #2452, #16546 ) ;
#3739 = AXIS2_PLACEMENT_3D ( 'NONE', #13593, #12017, #6372 ) ;
#3740 = PLANE ( 'NONE',  #1073 ) ;
#3741 = CARTESIAN_POINT ( 'NONE',  ( -5.330712181944245322E-15, -29.39828321677494216, -9.160639286973687234 ) ) ;
#3742 = DIRECTION ( 'NONE',  ( 0.000000000000000000, -1.224646799147353207E-16, 1.000000000000000000 ) ) ;
#3743 = CARTESIAN_POINT ( 'NONE',  ( 4.499999999999999112, 26.74680007765647360, -0.05647727720537982360 ) ) ;
#3744 = CARTESIAN_POINT ( 'NONE',  ( -1.071796769724486786, -23.08030267449302286, -15.65439537464544806 ) ) ;
#3745 = CARTESIAN_POINT ( 'NONE',  ( 9.000000000000001776, 34.19999999999999574, -2.500000000000002665 ) ) ;
#3746 = CIRCLE ( 'NONE', #11719, 0.9999999999999991118 ) ;
#3747 = CARTESIAN_POINT ( 'NONE',  ( -2.121784821874996396, -19.09383943047100018, -9.394583823722271632 ) ) ;
#3748 = VERTEX_POINT ( 'NONE', #5718 ) ;
#3749 = DIRECTION ( 'NONE',  ( -0.000000000000000000, -0.5735764363510414965, -0.8191520442889950182 ) ) ;
#3750 = PLANE ( 'NONE',  #5313 ) ;
#3751 = DIRECTION ( 'NONE',  ( 3.469446951953612217E-16, 0.000000000000000000, 1.000000000000000000 ) ) ;
#3752 = CARTESIAN_POINT ( 'NONE',  ( 1.989345975306426206, 33.99680007765647360, -1.515154207786343799 ) ) ;
#3753 = CARTESIAN_POINT ( 'NONE',  ( 9.000000000000000000, 40.79999999999999716, -2.500000000000001332 ) ) ;
#3754 = CARTESIAN_POINT ( 'NONE',  ( -0.05938372350927861865, 26.12180007765647716, -3.680117784833935701 ) ) ;
#3755 = CARTESIAN_POINT ( 'NONE',  ( 0.000000000000000000, 25.39999999999999503, 2.500000000000000000 ) ) ;
#3756 = ADVANCED_FACE ( 'NONE', ( #7000 ), #9964, .F. ) ;
#3757 = SHAPE_DEFINITION_REPRESENTATION ( #9300, #10770 ) ;
#3758 = FACE_OUTER_BOUND ( 'NONE', #268, .T. ) ;
#3759 = ADVANCED_FACE ( 'NONE', ( #2939 ), #5626, .T. ) ;
#3760 = ORIENTED_EDGE ( 'NONE', *, *, #6381, .T. ) ;
#3761 = CARTESIAN_POINT ( 'NONE',  ( -5.330712181944246111E-15, -25.01042347868948212, -2.894126148162874834 ) ) ;
#3762 = CARTESIAN_POINT ( 'NONE',  ( -1.027846397803541700, 27.49680007765648071, 3.346150245485522312 ) ) ;
#3763 = ORIENTED_EDGE ( 'NONE', *, *, #4008, .F. ) ;
#3764 = ADVANCED_FACE ( 'NONE', ( #10148 ), #11358, .F. ) ;
#3765 = CYLINDRICAL_SURFACE ( 'NONE', #4714, 2.149999999999995470 ) ;
#3766 = CARTESIAN_POINT ( 'NONE',  ( 1.998572135942813466, -24.18888450820426783, -16.52405203462232564 ) ) ;
#3767 = CARTESIAN_POINT ( 'NONE',  ( 7.573138360694985138, -10.32747394560775511, 6.453217690228979286 ) ) ;
#3768 = FACE_OUTER_BOUND ( 'NONE', #4722, .T. ) ;
#3769 = CARTESIAN_POINT ( 'NONE',  ( -4.243569643749997233, -23.94744319389470633, -14.19050330815125704 ) ) ;
#3770 = ORIENTED_EDGE ( 'NONE', *, *, #3041, .T. ) ;
#3771 = DIRECTION ( 'NONE',  ( 0.000000000000000000, 0.8191520442889952403, -0.5735764363510413855 ) ) ;
#3772 = CARTESIAN_POINT ( 'NONE',  ( 4.000000000000003553, -19.68015399097727069, -7.851010534249639683 ) ) ;
#3773 = CARTESIAN_POINT ( 'NONE',  ( 1.135272562821090458, 34.74680007765648071, 3.311245368580554072 ) ) ;
#3774 = ORIENTED_EDGE ( 'NONE', *, *, #5682, .F. ) ;
#3775 = VECTOR ( 'NONE', #5436, 1000.000000000000000 ) ;
#3776 = ORIENTED_EDGE ( 'NONE', *, *, #17630, .F. ) ;
#3777 = CARTESIAN_POINT ( 'NONE',  ( 3.579096709490575479E-14, -25.70887743576973605, -5.460814815566567226 ) ) ;
#3778 =( NAMED_UNIT ( * ) PLANE_ANGLE_UNIT ( ) SI_UNIT ( $, .RADIAN. ) );
#3779 = CARTESIAN_POINT ( 'NONE',  ( 2.829195390882724759, 35.37819992234354061, -3.793023760679264278 ) ) ;
#3780 = CARTESIAN_POINT ( 'NONE',  ( 4.000000000000000888, -23.59376154151967953, -9.413903449649181354 ) ) ;
#3781 = EDGE_CURVE ( 'NONE', #15771, #6047, #15121, .T. ) ;
#3782 = CARTESIAN_POINT ( 'NONE',  ( -0.8262555684460826111, 26.50319992234354771, 2.360188852285421302 ) ) ;
#3783 = VERTEX_POINT ( 'NONE', #12664 ) ;
#3784 = CARTESIAN_POINT ( 'NONE',  ( -2.733110507866247652, 25.12180007765648071, 3.862833514489154574 ) ) ;
#3785 = CARTESIAN_POINT ( 'NONE',  ( -2.000000000000005773, -23.42011117034160605, -3.126428157563360344 ) ) ;
#3786 = ORIENTED_EDGE ( 'NONE', *, *, #15552, .T. ) ;
#3787 = CARTESIAN_POINT ( 'NONE',  ( 0.000000000000000000, 0.7216878364870329410, 1.249999999999999778 ) ) ;
#3788 = AXIS2_PLACEMENT_3D ( 'NONE', #6165, #4773, #17224 ) ;
#3789 = DIRECTION ( 'NONE',  ( 1.000000000000000000, 0.000000000000000000, 0.000000000000000000 ) ) ;
#3790 = LINE ( 'NONE', #15115, #18269 ) ;
#3791 = CARTESIAN_POINT ( 'NONE',  ( 4.243569643749997233, -21.89576011715183057, -2.717415988351541412 ) ) ;
#3792 = CARTESIAN_POINT ( 'NONE',  ( -2.121784821874996396, -20.67475948316355883, -11.65237164579381535 ) ) ;
#3793 = LINE ( 'NONE', #9355, #17145 ) ;
#3794 = ORIENTED_EDGE ( 'NONE', *, *, #16427, .F. ) ;
#3795 = CARTESIAN_POINT ( 'NONE',  ( -8.500000000000010658, 15.00000000000000178, 22.64999999999998437 ) ) ;
#3796 = CARTESIAN_POINT ( 'NONE',  ( -2.211161402132901799, 15.87180007765647716, -2.942372952327172886 ) ) ;
#3797 = SURFACE_STYLE_FILL_AREA ( #16710 ) ;
#3798 = CARTESIAN_POINT ( 'NONE',  ( -4.243569643749997233, -24.23781626479742712, -14.60519903057256208 ) ) ;
#3799 = EDGE_LOOP ( 'NONE', ( #15244, #1011, #13623, #17796 ) ) ;
#3800 = MECHANICAL_DESIGN_GEOMETRIC_PRESENTATION_REPRESENTATION (  '', ( #563 ), #254 ) ;
#3801 = CARTESIAN_POINT ( 'NONE',  ( -0.05938372350920063936, 31.37819992234354416, 3.680117784833935701 ) ) ;
#3802 = CARTESIAN_POINT ( 'NONE',  ( 2.115076519116425580, 21.12819992234354061, 3.012182706137062294 ) ) ;
#3803 = CARTESIAN_POINT ( 'NONE',  ( -4.243569643749997233, -17.75281768130346194, -5.343661229830111381 ) ) ;
#3804 = CARTESIAN_POINT ( 'NONE',  ( 1.593127413382998903, 29.62180007765647716, 2.091722143975139669 ) ) ;
#3805 = CARTESIAN_POINT ( 'NONE',  ( -0.05938372350918959958, 23.87819992234354416, 4.731580009072201776 ) ) ;
#3806 = UNCERTAINTY_MEASURE_WITH_UNIT (LENGTH_MEASURE( 1.000000000000000082E-05 ), #14295, 'distance_accuracy_value', 'NONE');
#3807 = CARTESIAN_POINT ( 'NONE',  ( -5.279047395330986450E-15, -28.21611830590294190, -7.962677234997037168 ) ) ;
#3808 = VERTEX_POINT ( 'NONE', #15827 ) ;
#3809 = CARTESIAN_POINT ( 'NONE',  ( -9.000000000000003553, 25.39999999999999503, -2.500000000000001776 ) ) ;
#3810 = CARTESIAN_POINT ( 'NONE',  ( 1.336863392178479160, 36.24680007765647360, -4.297206761780677731 ) ) ;
#3811 = FACE_OUTER_BOUND ( 'NONE', #3853, .T. ) ;
#3812 = AXIS2_PLACEMENT_3D ( 'NONE', #354, #10160, #7285 ) ;
#3813 = CARTESIAN_POINT ( 'NONE',  ( -2.121784821874996396, -21.67493339405068653, -13.08076802302275077 ) ) ;
#3814 = AXIS2_PLACEMENT_3D ( 'NONE', #95, #10085, #3437 ) ;
#3815 = CARTESIAN_POINT ( 'NONE',  ( -1.071796769724491671, -22.82219327813506737, -15.28577695471540210 ) ) ;
#3816 = DIRECTION ( 'NONE',  ( -0.000000000000000000, 0.5000000000000000000, 0.8660254037844385966 ) ) ;
#3817 = CYLINDRICAL_SURFACE ( 'NONE', #18336, 0.9999999999999991118 ) ;
#3818 = ORIENTED_EDGE ( 'NONE', *, *, #12155, .T. ) ;
#3819 = ORIENTED_EDGE ( 'NONE', *, *, #14291, .F. ) ;
#3820 = CARTESIAN_POINT ( 'NONE',  ( 2.864755990943265829, 16.99680007765647716, 2.011557305968487697 ) ) ;
#3821 = DIRECTION ( 'NONE',  ( -1.000000000000000000, -0.000000000000000000, -0.000000000000000000 ) ) ;
#3822 = EDGE_CURVE ( 'NONE', #5909, #6012, #6302, .T. ) ;
#3823 = DIRECTION ( 'NONE',  ( -6.162975822039154730E-33, 0.5735764363510414965, 0.8191520442889950182 ) ) ;
#3824 = DIRECTION ( 'NONE',  ( -0.7601375407242620952, -0.6497622020259954390, 0.000000000000000000 ) ) ;
#3825 = EDGE_LOOP ( 'NONE', ( #4853, #15736, #14077, #7623 ) ) ;
#3826 = CARTESIAN_POINT ( 'NONE',  ( -1.989345975306457071, 34.75319992234354771, -1.515154207786300944 ) ) ;
#3827 = CARTESIAN_POINT ( 'NONE',  ( 4.730628863548789710E-15, -19.66053299056463288, -12.33965115782429400 ) ) ;
#3828 = CARTESIAN_POINT ( 'NONE',  ( 1.135272562821090458, 32.24680007765648071, 3.311245368580554072 ) ) ;
#3829 = EDGE_CURVE ( 'NONE', #17541, #1681, #6285, .T. ) ;
#3830 = AXIS2_PLACEMENT_3D ( 'NONE', #13961, #15187, #1274 ) ;
#3831 = CARTESIAN_POINT ( 'NONE',  ( 2.864755990943222308, 23.00319992234354416, -2.011557305968548093 ) ) ;
#3832 = LINE ( 'NONE', #13561, #117 ) ;
#3834 = ADVANCED_FACE ( 'NONE', ( #14058 ), #16372, .T. ) ;
#3833 = TOROIDAL_SURFACE ( 'NONE', #18362, 9.000000000000001776, 0.9999999999999991118 ) ;
#3835 = CARTESIAN_POINT ( 'NONE',  ( -9.000000000000003553, 20.99999999999999289, -2.500000000000001776 ) ) ;
#3836 = CARTESIAN_POINT ( 'NONE',  ( 2.121784821874994176, -27.08275518420459349, -7.989467598523504854 ) ) ;
#3837 = AXIS2_PLACEMENT_3D ( 'NONE', #11609, #8636, #36 ) ;
#3838 = CARTESIAN_POINT ( 'NONE',  ( -13.00000000000000178, 49.00000000000000000, -16.00000000000000000 ) ) ;
#3839 = CARTESIAN_POINT ( 'NONE',  ( -4.481649420246366589, 20.37180007765648071, 1.518615910253458878 ) ) ;
#3840 = AXIS2_PLACEMENT_3D ( 'NONE', #4204, #14033, #15527 ) ;
#3841 = FACE_OUTER_BOUND ( 'NONE', #13740, .T. ) ;
#3842 = DIRECTION ( 'NONE',  ( -1.000000000000000000, 0.000000000000000000, 0.000000000000000000 ) ) ;
#3843 =( BOUNDED_CURVE ( )  B_SPLINE_CURVE ( 2, ( #3237, #453, #18216, #11220, #1412, #3137, #7042, #6001, #4708 ),
 .UNSPECIFIED., .F., .F. ) 
 B_SPLINE_CURVE_WITH_KNOTS ( ( 3, 2, 2, 2, 3 ),
 ( 0.6465517241379310498, 0.6494252873563218786, 0.6551724137931034253, 0.6609195402298850830, 0.6637931034482759118 ),
 .UNSPECIFIED. ) 
 CURVE ( )  GEOMETRIC_REPRESENTATION_ITEM ( )  RATIONAL_B_SPLINE_CURVE ( ( 0.9330127018922194093, 0.9330127018922194093, 1.000000000000000000, 0.8660254037844387076, 1.000000000000000000, 0.8660254037844387076, 1.000000000000000000, 0.9330127018922180770, 0.9330127018922194093 ) ) 
 REPRESENTATION_ITEM ( '' )  );
#3844 = CARTESIAN_POINT ( 'NONE',  ( -4.243569643750005227, -24.56289054618417111, -6.526472994295373198 ) ) ;
#3845 = ORIENTED_EDGE ( 'NONE', *, *, #4725, .T. ) ;
#3846 = CARTESIAN_POINT ( 'NONE',  ( 1.533898589781675205E-14, -28.03186200299146336, -8.778380594936995962 ) ) ;
#3847 = CARTESIAN_POINT ( 'NONE',  ( 2.000000000000004441, -22.32630111707070242, -13.64325923146567199 ) ) ;
#3848 = CARTESIAN_POINT ( 'NONE',  ( -0.7188294034286043521, 34.99680007765648071, 2.395093729190366005 ) ) ;
#3849 = DIRECTION ( 'NONE',  ( 1.000000000000000000, 0.000000000000000000, 0.000000000000000000 ) ) ;
#3850 = CARTESIAN_POINT ( 'NONE',  ( 3.481649420246370141, 34.12180007765648071, -1.193696214020541602 ) ) ;
#3851 = CARTESIAN_POINT ( 'NONE',  ( -4.000000000000000888, -20.10928469068709745, -4.437554780593541359 ) ) ;
#3852 = DIRECTION ( 'NONE',  ( 0.000000000000000000, -0.000000000000000000, -1.000000000000000000 ) ) ;
#3853 = EDGE_LOOP ( 'NONE', ( #17157, #18021, #8464, #5830 ) ) ;
#3854 = CARTESIAN_POINT ( 'NONE',  ( -4.243569643749998122, -18.81751894128008473, -6.864212212041559624 ) ) ;
#3855 = AXIS2_PLACEMENT_3D ( 'NONE', #1522, #1610, #4379 ) ;
#3856 = CARTESIAN_POINT ( 'NONE',  ( -3.481649420246369697, 25.37180007765648071, 1.193696214020542490 ) ) ;
#3857 = ORIENTED_EDGE ( 'NONE', *, *, #5186, .F. ) ;
#3858 = CARTESIAN_POINT ( 'NONE',  ( 0.000000000000000000, 5.977523610840987267, 32.81826849749789687 ) ) ;
#3859 = CARTESIAN_POINT ( 'NONE',  ( 0.000000000000000000, 5.000000000000000000, 0.000000000000000000 ) ) ;
#3860 = CARTESIAN_POINT ( 'NONE',  ( 0.2152313249818218199, -23.77077346268850988, -16.79000057782539201 ) ) ;
#3861 = DIRECTION ( 'NONE',  ( -3.373073425510457965E-16, 0.000000000000000000, -1.000000000000000000 ) ) ;
#3862 = DIRECTION ( 'NONE',  ( 0.000000000000000000, 0.000000000000000000, -1.000000000000000000 ) ) ;
#3863 = CARTESIAN_POINT ( 'NONE',  ( 4.243569643750003451, -24.54969845206331058, -15.05061295465469762 ) ) ;
#3864 = EDGE_CURVE ( 'NONE', #16968, #12341, #15668, .T. ) ;
#3865 = EDGE_LOOP ( 'NONE', ( #10369, #5746, #8317, #17045 ) ) ;
#3866 = CARTESIAN_POINT ( 'NONE',  ( 1.300000000000000044, 0.000000000000000000, 0.000000000000000000 ) ) ;
#3867 = CARTESIAN_POINT ( 'NONE',  ( -4.000000000000004441, -23.33460051901814225, -5.017465244859820039 ) ) ;
#3868 = AXIS2_PLACEMENT_3D ( 'NONE', #8631, #4473, #7243 ) ;
#3869 = CARTESIAN_POINT ( 'NONE',  ( -0.8262555684461330152, 18.49680007765647716, -2.360188852285403982 ) ) ;
#3870 = ORIENTED_EDGE ( 'NONE', *, *, #1917, .T. ) ;
#3871 = EDGE_LOOP ( 'NONE', ( #9992, #15272, #1948, #15222 ) ) ;
#3872 = DIRECTION ( 'NONE',  ( -0.000000000000000000, -1.000000000000000000, -0.000000000000000000 ) ) ;
#3873 =( LENGTH_UNIT ( ) NAMED_UNIT ( * ) SI_UNIT ( .MILLI., .METRE. ) );
#3874 = CARTESIAN_POINT ( 'NONE',  ( -3.673772985318163098, 34.25319992234354061, 2.599342558261029001 ) ) ;
#3875 = CARTESIAN_POINT ( 'NONE',  ( 8.000000000000005329, 27.59999999999999432, 2.499999999999997780 ) ) ;
#3876 = CARTESIAN_POINT ( 'NONE',  ( 1.989345975306457071, 28.50319992234355126, 1.515154207786300500 ) ) ;
#3877 = ORIENTED_EDGE ( 'NONE', *, *, #15787, .F. ) ;
#3878 = CARTESIAN_POINT ( 'NONE',  ( 4.730628863548789710E-15, -21.49956243961516122, -14.96605739982588368 ) ) ;
#3879 = CARTESIAN_POINT ( 'NONE',  ( 4.518350579753633411, 24.37180007765647005, 1.405661355842698468 ) ) ;
#3880 = CARTESIAN_POINT ( 'NONE',  ( -4.000000000000000888, -21.14172227611897270, -5.912028460313731415 ) ) ;
#3881 = ORIENTED_EDGE ( 'NONE', *, *, #6478, .F. ) ;
#3882 = CARTESIAN_POINT ( 'NONE',  ( -1.071796769724486786, -20.82184545706574852, -12.42898420126429748 ) ) ;
#3883 = VECTOR ( 'NONE', #15541, 1000.000000000000000 ) ;
#3884 = ADVANCED_FACE ( 'NONE', ( #246 ), #17266, .F. ) ;
#3885 = DIRECTION ( 'NONE',  ( -1.000000000000000000, -0.000000000000000000, -0.000000000000000000 ) ) ;
#3886 = CARTESIAN_POINT ( 'NONE',  ( 2.121784821875004390, -17.07198249233357856, -6.507072867603563182 ) ) ;
#3887 = EDGE_CURVE ( 'NONE', #6155, #12907, #639, .T. ) ;
#3888 = CARTESIAN_POINT ( 'NONE',  ( -4.243569643750000786, -22.09350067554145625, -7.271308884309165776 ) ) ;
#3889 = EDGE_CURVE ( 'NONE', #8328, #2307, #17637, .T. ) ;
#3890 = DIRECTION ( 'NONE',  ( 1.000000000000000000, 0.000000000000000000, 0.000000000000000000 ) ) ;
#3891 = ORIENTED_EDGE ( 'NONE', *, *, #3889, .T. ) ;
#3892 = CARTESIAN_POINT ( 'NONE',  ( -2.000000000000005773, -27.35627946550557255, -8.747859062503353655 ) ) ;
#3893 = FACE_OUTER_BOUND ( 'NONE', #8826, .T. ) ;
#3894 = CARTESIAN_POINT ( 'NONE',  ( -3.500000000000000444, 15.49680007765647893, 0.05647727720536901974 ) ) ;
#3895 =( LENGTH_UNIT ( ) NAMED_UNIT ( * ) SI_UNIT ( .MILLI., .METRE. ) );
#3896 = ORIENTED_EDGE ( 'NONE', *, *, #12152, .T. ) ;
#3897 = CIRCLE ( 'NONE', #654, 10.00000000000000178 ) ;
#3898 = CARTESIAN_POINT ( 'NONE',  ( -3.481649420246394122, 37.12819992234354771, -1.193696214020467883 ) ) ;
#3899 = CARTESIAN_POINT ( 'NONE',  ( 0.05938372350920110426, 20.12819992234354061, -3.680117784833935701 ) ) ;
#3900 = CARTESIAN_POINT ( 'NONE',  ( -2.000000000000005773, -29.67926403272728919, -12.06542484187378506 ) ) ;
#3901 = CARTESIAN_POINT ( 'NONE',  ( -2.500000000000001332, 27.99680007765648426, 0.05647727720535858364 ) ) ;
#3902 = CARTESIAN_POINT ( 'NONE',  ( 4.499999999999999112, 28.25319992234354416, 0.05647727720528474687 ) ) ;
#3903 = CARTESIAN_POINT ( 'NONE',  ( -1.999999999999996225, -21.96064613819196154, -13.12104980222467532 ) ) ;
#3904 = ORIENTED_EDGE ( 'NONE', *, *, #7785, .T. ) ;
#3905 = CARTESIAN_POINT ( 'NONE',  ( 0.000000000000000000, -3.999999999999991562, 11.59510085796834566 ) ) ;
#3906 = CARTESIAN_POINT ( 'NONE',  ( 2.733110507866247652, 38.87180007765646650, -3.862833514489153686 ) ) ;
#3907 = DIRECTION ( 'NONE',  ( 0.000000000000000000, 0.000000000000000000, 1.000000000000000000 ) ) ;
#3908 = CARTESIAN_POINT ( 'NONE',  ( -4.243569643750000786, -23.86800277550248950, -9.805560521328242629 ) ) ;
#3909 = CARTESIAN_POINT ( 'NONE',  ( -1.999999999999996225, -17.83089579646446410, -7.223155083343911542 ) ) ;
#3910 = DIRECTION ( 'NONE',  ( 0.000000000000000000, 0.000000000000000000, 1.000000000000000000 ) ) ;
#3911 = CYLINDRICAL_SURFACE ( 'NONE', #16250, 2.149999999999995470 ) ;
#3912 = VERTEX_POINT ( 'NONE', #4688 ) ;
#3913 = ORIENTED_EDGE ( 'NONE', *, *, #4609, .F. ) ;
#3914 = CARTESIAN_POINT ( 'NONE',  ( 3.500000000000000444, 16.74680007765647716, -0.05647727720536935281 ) ) ;
#3915 = DIRECTION ( 'NONE',  ( -1.000000000000000000, -0.000000000000000000, -0.000000000000000000 ) ) ;
#3916 = AXIS2_PLACEMENT_3D ( 'NONE', #192, #17006, #5842 ) ;
#3917 = CARTESIAN_POINT ( 'NONE',  ( 1.071796769724476128, -18.26380489492371595, -8.775723671275654780 ) ) ;
#3918 = DIRECTION ( 'NONE',  ( -0.5735764363510413855, 0.6710100716628397688, -0.4698463103929523266 ) ) ;
#3919 = VERTEX_POINT ( 'NONE', #14912 ) ;
#3920 = CARTESIAN_POINT ( 'NONE',  ( -0.05938372350921170689, 33.87819992234354061, 2.628655560595669183 ) ) ;
#3921 = CARTESIAN_POINT ( 'NONE',  ( 4.730628863548789710E-15, -20.69297057599650813, -13.81412483754448495 ) ) ;
#3922 = CARTESIAN_POINT ( 'NONE',  ( 2.115076519116362963, 33.87180007765648071, -3.012182706137107147 ) ) ;
#3923 =( GEOMETRIC_REPRESENTATION_CONTEXT ( 3 ) GLOBAL_UNCERTAINTY_ASSIGNED_CONTEXT ( ( #10851 ) ) GLOBAL_UNIT_ASSIGNED_CONTEXT ( ( #8221, #13885, #5444 ) ) REPRESENTATION_CONTEXT ( 'NONE', 'WORKASPACE' ) );
#3924 = CARTESIAN_POINT ( 'NONE',  ( -1.135272562821019626, 24.00319992234354416, 3.311245368580577164 ) ) ;
#3925 = CARTESIAN_POINT ( 'NONE',  ( 8.500000000000019540, -1.201721234452885367, 20.49999999999998934 ) ) ;
#3926 = CARTESIAN_POINT ( 'NONE',  ( 8.500000000000001776, 14.99364916731036956, -22.64999999999999147 ) ) ;
#3927 = CARTESIAN_POINT ( 'NONE',  ( 4.243569643750003451, -21.74275876667039853, -11.04188763791542804 ) ) ;
#3928 = TOROIDAL_SURFACE ( 'NONE', #14594, 9.000000000000003553, 0.9999999999999991118 ) ;
#3929 = COLOUR_RGB ( '',0.8941176470588234615, 0.8941176470588234615, 0.8941176470588234615 ) ;
#3930 = ADVANCED_FACE ( 'NONE', ( #9230 ), #2206, .F. ) ;
#3931 = CARTESIAN_POINT ( 'NONE',  ( 1.336863392178479160, 23.74680007765647716, -4.297206761780677731 ) ) ;
#3932 = CYLINDRICAL_SURFACE ( 'NONE', #17506, 6.000000000000000000 ) ;
#3933 = FACE_OUTER_BOUND ( 'NONE', #1021, .T. ) ;
#3934 = CARTESIAN_POINT ( 'NONE',  ( 4.730628863548789710E-15, -17.85376721605885209, -9.759322218313958075 ) ) ;
#3935 = EDGE_CURVE ( 'NONE', #5777, #8773, #1829, .T. ) ;
#3936 = CARTESIAN_POINT ( 'NONE',  ( 4.000000000000000000, 0.000000000000000000, 0.000000000000000000 ) ) ;
#3937 = FACE_OUTER_BOUND ( 'NONE', #2867, .T. ) ;
#3938 = CARTESIAN_POINT ( 'NONE',  ( 2.481649420246374138, 39.12180007765647360, -0.8687765177876252132 ) ) ;
#3939 = CARTESIAN_POINT ( 'NONE',  ( -1.734723475976807094E-15, 23.19999999999999574, -11.50000000000000178 ) ) ;
#3940 = CARTESIAN_POINT ( 'NONE',  ( 1.135272562821090458, 37.24680007765648071, 3.311245368580554072 ) ) ;
#3941 = CARTESIAN_POINT ( 'NONE',  ( -1.071796769724481457, -22.04786508906114761, -14.17992169492525889 ) ) ;
#3942 = VECTOR ( 'NONE', #13951, 1000.000000000000000 ) ;
#3943 = ITEM_DEFINED_TRANSFORMATION ( 'NONE', 'NONE', #13392,  #16940 ) ;
#3944 = AXIS2_PLACEMENT_3D ( 'NONE', #17372, #10383, #9272 ) ;
#3945 = CARTESIAN_POINT ( 'NONE',  ( -2.054657775866485014, 15.00000000000001243, -3.211012929026491047 ) ) ;
#3946 = ORIENTED_EDGE ( 'NONE', *, *, #9880, .T. ) ;
#3947 = CARTESIAN_POINT ( 'NONE',  ( 4.243569643749997233, -23.73478956620236957, -5.343822230353133307 ) ) ;
#3948 = CARTESIAN_POINT ( 'NONE',  ( -3.518350579753630747, 20.62180007765646650, -1.080741659609802729 ) ) ;
#3949 = DIRECTION ( 'NONE',  ( 0.000000000000000000, 0.000000000000000000, 1.000000000000000000 ) ) ;
#3950 = CARTESIAN_POINT ( 'NONE',  ( -4.243569643749998122, -24.46366198661065283, -14.92774014801135074 ) ) ;
#3951 = CIRCLE ( 'NONE', #709, 10.00000000000000000 ) ;
#3952 = CARTESIAN_POINT ( 'NONE',  ( 3.064183985264992582, -21.85725672082847382, -2.451266466499125052 ) ) ;
#3953 = ADVANCED_FACE ( 'NONE', ( #13402 ), #13488, .T. ) ;
#3954 = CARTESIAN_POINT ( 'NONE',  ( -2.000000000000005773, -23.67822056669957576, -3.495046577493408968 ) ) ;
#3955 = CARTESIAN_POINT ( 'NONE',  ( 4.243569643750003451, -24.29158905570534088, -14.68199453472465166 ) ) ;
#3956 = ORIENTED_EDGE ( 'NONE', *, *, #15559, .T. ) ;
#3957 = CARTESIAN_POINT ( 'NONE',  ( 8.000000000000005329, 29.79999999999999716, 2.499999999999997780 ) ) ;
#3958 = CARTESIAN_POINT ( 'NONE',  ( 4.000000000000000888, -21.07719492773443193, -5.819873856337981266 ) ) ;
#3959 = CARTESIAN_POINT ( 'NONE',  ( 0.7188294034286049072, 16.24680007765648071, -2.395093729190366005 ) ) ;
#3960 = ORIENTED_EDGE ( 'NONE', *, *, #9531, .T. ) ;
#3961 = CARTESIAN_POINT ( 'NONE',  ( -2.000000000000005773, -23.93632996305754190, -3.863664997423455816 ) ) ;
#3962 = SURFACE_STYLE_USAGE ( .BOTH. , #8481 ) ;
#3963 = CARTESIAN_POINT ( 'NONE',  ( -4.481649420246396787, 34.62819992234354771, -1.518615910253363399 ) ) ;
#3964 = CARTESIAN_POINT ( 'NONE',  ( 0.000000000000000000, 0.000000000000000000, 0.000000000000000000 ) ) ;
#3965 = CARTESIAN_POINT ( 'NONE',  ( 2.500000000000001332, 30.75319992234354416, 0.05647727720530566764 ) ) ;
#3966 = AXIS2_PLACEMENT_3D ( 'NONE', #10127, #8735, #606 ) ;
#3967 = ORIENTED_EDGE ( 'NONE', *, *, #4289, .F. ) ;
#3968 = CARTESIAN_POINT ( 'NONE',  ( -4.243569643750000786, -24.93270403547910874, -11.32611150353969087 ) ) ;
#3969 = CARTESIAN_POINT ( 'NONE',  ( -2.733110507866247652, 22.62180007765647360, 3.862833514489154574 ) ) ;
#3970 = CARTESIAN_POINT ( 'NONE',  ( 4.000000000000000888, -20.75455818158202703, -5.359100830418656258 ) ) ;
#3971 = EDGE_LOOP ( 'NONE', ( #17487, #15706, #12869, #4193 ) ) ;
#3972 = FACE_OUTER_BOUND ( 'NONE', #11222, .T. ) ;
#3973 = DIRECTION ( 'NONE',  ( 1.000000000000000000, 0.000000000000000000, 0.000000000000000000 ) ) ;
#3974 = DIRECTION ( 'NONE',  ( -1.000000000000000000, 0.000000000000000000, 4.336808689942021680E-16 ) ) ;
#3975 = CARTESIAN_POINT ( 'NONE',  ( 4.243569643749996345, -24.76722715163424127, -6.818295910073324251 ) ) ;
#3976 = EDGE_LOOP ( 'NONE', ( #17391, #409 ) ) ;
#3977 = PRODUCT ( 'socket button head screw_iso_ISO 7380 - M4 x 12 - 12N', 'socket button head screw_iso_ISO 7380 - M4 x 12 - 12N', '', ( #13489 ) ) ;
#3978 = DIRECTION ( 'NONE',  ( 1.000000000000000000, 0.000000000000000000, 0.000000000000000000 ) ) ;
#3979 = EDGE_LOOP ( 'NONE', ( #12829, #8789, #9971, #13310, #18277, #15752, #7206, #3877, #1962 ) ) ;
#3980 = CARTESIAN_POINT ( 'NONE',  ( -1.999999999999996225, -20.99273590255452149, -11.73873072849375987 ) ) ;
#3981 = AXIS2_PLACEMENT_3D ( 'NONE', #8262, #18122, #18297 ) ;
#3982 = CARTESIAN_POINT ( 'NONE',  ( 4.000000000000000888, -25.14241791966749417, -11.62561396922946777 ) ) ;
#3983 = DIRECTION ( 'NONE',  ( 0.000000000000000000, 0.000000000000000000, -1.000000000000000000 ) ) ;
#3984 = ORIENTED_EDGE ( 'NONE', *, *, #16350, .F. ) ;
#3985 = CARTESIAN_POINT ( 'NONE',  ( -2.115076519116425580, 34.87819992234354771, -3.012182706137062738 ) ) ;
#3986 = CARTESIAN_POINT ( 'NONE',  ( -3.518350579753606322, 16.87819992234354061, 1.080741659609877781 ) ) ;
#3987 = CARTESIAN_POINT ( 'NONE',  ( 2.121784821875004390, -17.33009188869154826, -6.875691287533610918 ) ) ;
#3988 = CARTESIAN_POINT ( 'NONE',  ( 2.500000000000001332, 31.74680007765648782, -0.05647727720535888202 ) ) ;
#3989 = EDGE_CURVE ( 'NONE', #4032, #3136, #1932, .T. ) ;
#3990 = CIRCLE ( 'NONE', #12545, 2.149999999999995470 ) ;
#3991 = CARTESIAN_POINT ( 'NONE',  ( -2.829195390882724315, 24.12819992234354771, 3.793023760679264722 ) ) ;
#3992 = ADVANCED_FACE ( 'NONE', ( #10241 ), #16112, .T. ) ;
#3993 = CARTESIAN_POINT ( 'NONE',  ( -2.000000000000005773, -27.80797090842707320, -9.392941296374171856 ) ) ;
#3994 = ORIENTED_EDGE ( 'NONE', *, *, #12650, .F. ) ;
#3995 = ADVANCED_FACE ( 'NONE', ( #13125 ), #11635, .T. ) ;
#3996 = CARTESIAN_POINT ( 'NONE',  ( 2.121784821875004390, -16.84613677052036351, -6.184531750164772745 ) ) ;
#3997 = CARTESIAN_POINT ( 'NONE',  ( -1.135272562821090014, 25.99680007765648071, -3.311245368580554072 ) ) ;
#3998 = FILL_AREA_STYLE_COLOUR ( '', #8718 ) ;
#3999 = EDGE_CURVE ( 'NONE', #16392, #8328, #17022, .T. ) ;
#4000 = CARTESIAN_POINT ( 'NONE',  ( -4.243569643749998122, -20.85013043759908413, -9.767082268990684213 ) ) ;
#4001 = CARTESIAN_POINT ( 'NONE',  ( -4.000000000000004441, -27.91604230366714390, -11.56044219761139935 ) ) ;
#4002 = CARTESIAN_POINT ( 'NONE',  ( 9.000000000000005329, 20.99999999999999289, 2.499999999999997335 ) ) ;
#4003 = DIRECTION ( 'NONE',  ( -1.000000000000000000, 0.000000000000000000, 4.336808689942021680E-16 ) ) ;
#4004 = ORIENTED_EDGE ( 'NONE', *, *, #15347, .F. ) ;
#4005 = ORIENTED_EDGE ( 'NONE', *, *, #7028, .T. ) ;
#4006 = SHAPE_REPRESENTATION ( 'armature', ( #16940 ), #1250 ) ;
#4007 = CARTESIAN_POINT ( 'NONE',  ( 1.027846397803542144, 16.24680007765647716, -3.346150245485522312 ) ) ;
#4008 = EDGE_CURVE ( 'NONE', #16065, #5051, #8115, .T. ) ;
#4009 = CARTESIAN_POINT ( 'NONE',  ( -4.000000000000004441, -23.78629196193964646, -5.662547478730638240 ) ) ;
#4010 = DIRECTION ( 'NONE',  ( 0.000000000000000000, 0.000000000000000000, 1.000000000000000000 ) ) ;
#4011 = FACE_OUTER_BOUND ( 'NONE', #1462, .T. ) ;
#4012 = ORIENTED_EDGE ( 'NONE', *, *, #12319, .F. ) ;
#4013 = CARTESIAN_POINT ( 'NONE',  ( -2.055738996568281518, 36.75319992234354771, 1.423772053676066962 ) ) ;
#4014 = CARTESIAN_POINT ( 'NONE',  ( -4.243569643750000786, -24.38422156821842535, -10.54279736118833988 ) ) ;
#4015 = CARTESIAN_POINT ( 'NONE',  ( 3.500000000000000444, 34.24680007765648071, -0.05647727720536935281 ) ) ;
#4016 = CARTESIAN_POINT ( 'NONE',  ( -2.211161402132839182, 29.12819992234354771, 2.942372952327218627 ) ) ;
#4017 = FACE_OUTER_BOUND ( 'NONE', #7449, .T. ) ;
#4018 = VECTOR ( 'NONE', #5589, 1000.000000000000000 ) ;
#4019 = CARTESIAN_POINT ( 'NONE',  ( -4.243569643750000786, -24.15837584640520674, -10.22025624374954766 ) ) ;
#4020 = CARTESIAN_POINT ( 'NONE',  ( 8.500000000000001776, 10.00000000000000000, -20.49999999999999645 ) ) ;
#4021 = DIRECTION ( 'NONE',  ( 1.000000000000000000, 0.000000000000000000, 0.000000000000000000 ) ) ;
#4022 = CARTESIAN_POINT ( 'NONE',  ( -13.00000000000000178, 15.00000000000000178, -25.00000000000000355 ) ) ;
#4023 = CARTESIAN_POINT ( 'NONE',  ( 2.121784821875004390, -18.62063887048139321, -8.718783387183849598 ) ) ;
#4024 = VECTOR ( 'NONE', #1603, 1000.000000000000000 ) ;
#4025 = CARTESIAN_POINT ( 'NONE',  ( -4.000000000000000888, -21.98057781498731345, -7.110038326093152783 ) ) ;
#4026 =( NAMED_UNIT ( * ) PLANE_ANGLE_UNIT ( ) SI_UNIT ( $, .RADIAN. ) );
#4027 = CARTESIAN_POINT ( 'NONE',  ( 1.497042530366477164, 36.37180007765648071, -2.161531897785062384 ) ) ;
#4028 = AXIS2_PLACEMENT_3D ( 'NONE', #5994, #14351, #7199 ) ;
#4029 = CARTESIAN_POINT ( 'NONE',  ( -2.798362969681365886, 35.24680007765648071, 2.102939460078824929 ) ) ;
#4030 = CARTESIAN_POINT ( 'NONE',  ( -4.000000000000004441, -27.14171411459323835, -10.45458693782125792 ) ) ;
#4031 = CARTESIAN_POINT ( 'NONE',  ( 0.000000000000000000, 40.79999999999999716, 2.500000000000000000 ) ) ;
#4032 = VERTEX_POINT ( 'NONE', #14533 ) ;
#4033 = CARTESIAN_POINT ( 'NONE',  ( 4.243569643750000786, -21.70633658100450702, -6.718381254414091508 ) ) ;
#4034 = CARTESIAN_POINT ( 'NONE',  ( -0.05938372350927861171, 21.12180007765648071, -3.680117784833935701 ) ) ;
#4035 = VECTOR ( 'NONE', #15160, 1000.000000000000000 ) ;
#4036 = CARTESIAN_POINT ( 'NONE',  ( 2.121784821875004390, -24.04093619399873560, -16.45977020571485028 ) ) ;
#4037 = CYLINDRICAL_SURFACE ( 'NONE', #15400, 0.9999999999999991118 ) ;
#4038 = CARTESIAN_POINT ( 'NONE',  ( 8.499999999999992895, 14.80000000000000071, 22.69999999999999929 ) ) ;
#4039 = CARTESIAN_POINT ( 'NONE',  ( 2.121784821875004390, -22.75038921220889065, -14.61667810606461337 ) ) ;
#4040 = ORIENTED_EDGE ( 'NONE', *, *, #1119, .T. ) ;
#4041 = CARTESIAN_POINT ( 'NONE',  ( 1.999999999999994449, -24.47405787284159828, -4.631620039951150680 ) ) ;
#4042 = CARTESIAN_POINT ( 'NONE',  ( -2.864755990943265829, 35.74680007765648071, -2.011557305968488141 ) ) ;
#4043 = ORIENTED_EDGE ( 'NONE', *, *, #379, .F. ) ;
#4044 = FACE_OUTER_BOUND ( 'NONE', #4802, .T. ) ;
#4045 = ADVANCED_FACE ( 'NONE', ( #6174 ), #13312, .F. ) ;
#4046 = FILL_AREA_STYLE ('',( #4145 ) ) ;
#4047 = CARTESIAN_POINT ( 'NONE',  ( 1.336863392178569754, 38.75319992234354061, 4.297206761780648421 ) ) ;
#4048 = AXIS2_PLACEMENT_3D ( 'NONE', #13090, #406, #4652 ) ;
#4049 = CARTESIAN_POINT ( 'NONE',  ( -1.497042530366522461, 27.37819992234355126, -2.161531897785030409 ) ) ;
#4050 = ORIENTED_EDGE ( 'NONE', *, *, #8689, .T. ) ;
#4051 = CARTESIAN_POINT ( 'NONE',  ( 2.121784821875004390, -22.26643409403770590, -13.92551856869577342 ) ) ;
#4052 = CARTESIAN_POINT ( 'NONE',  ( -4.518350579753632523, 28.12180007765647716, -1.405661355842698468 ) ) ;
#4053 = EDGE_CURVE ( 'NONE', #10497, #7716, #9524, .T. ) ;
#4054 = CARTESIAN_POINT ( 'NONE',  ( 2.000000000000004441, -17.09958584011689098, -6.178736226875440884 ) ) ;
#4055 = ORIENTED_EDGE ( 'NONE', *, *, #4008, .T. ) ;
#4056 = CARTESIAN_POINT ( 'NONE',  ( -2.000000000000005773, -24.45254875577348130, -4.600901837283550400 ) ) ;
#4057 = EDGE_CURVE ( 'NONE', #5987, #6584, #6922, .T. ) ;
#4058 =( NAMED_UNIT ( * ) PLANE_ANGLE_UNIT ( ) SI_UNIT ( $, .RADIAN. ) );
#4059 = CARTESIAN_POINT ( 'NONE',  ( 8.000000000000005329, 18.79999999999999361, 2.499999999999997780 ) ) ;
#4060 = AXIS2_PLACEMENT_3D ( 'NONE', #17916, #2335, #5185 ) ;
#4061 = DIRECTION ( 'NONE',  ( 0.000000000000000000, 0.000000000000000000, 1.000000000000000000 ) ) ;
#4062 = VECTOR ( 'NONE', #16950, 1000.000000000000000 ) ;
#4063 = CARTESIAN_POINT ( 'NONE',  ( 4.243569643750000786, -22.73877416643638227, -8.192854934134281564 ) ) ;
#4064 = EDGE_LOOP ( 'NONE', ( #3599, #15378, #2449, #12860 ) ) ;
#4065 = PLANE ( 'NONE',  #3183 ) ;
#4066 = VERTEX_POINT ( 'NONE', #2568 ) ;
#4067 = CARTESIAN_POINT ( 'NONE',  ( -3.999999999999997335, -23.20764907453616743, -12.88879560662696200 ) ) ;
#4068 = DIRECTION ( 'NONE',  ( -0.000000000000000000, -0.5735764363510414965, -0.8191520442889950182 ) ) ;
#4069 =( NAMED_UNIT ( * ) PLANE_ANGLE_UNIT ( ) SI_UNIT ( $, .RADIAN. ) );
#4070 = CARTESIAN_POINT ( 'NONE',  ( 4.299564228933482956E-15, -22.57561058249592278, -14.93362036944126814 ) ) ;
#4071 = ORIENTED_EDGE ( 'NONE', *, *, #6036, .F. ) ;
#4072 = CARTESIAN_POINT ( 'NONE',  ( 1.135272562821020070, 35.25319992234354771, -3.311245368580577164 ) ) ;
#4073 = CARTESIAN_POINT ( 'NONE',  ( -1.027846397803611866, 20.00319992234354416, -3.346150245485499219 ) ) ;
#4074 = CARTESIAN_POINT ( 'NONE',  ( -4.000000000000000888, -25.59410936399887504, -12.27069620511382197 ) ) ;
#4075 = CARTESIAN_POINT ( 'NONE',  ( 2.481649420246374138, 31.62180007765648426, -0.8687765177876252132 ) ) ;
#4076 = EDGE_CURVE ( 'NONE', #13129, #6514, #11073, .T. ) ;
#4077 = AXIS2_PLACEMENT_3D ( 'NONE', #81, #14651, #12186 ) ;
#4078 = CARTESIAN_POINT ( 'NONE',  ( -0.05938372350918959958, 26.37819992234355126, 4.731580009072201776 ) ) ;
#4079 = CARTESIAN_POINT ( 'NONE',  ( -4.000000000000000888, -25.27147261784647014, -11.80992317919449519 ) ) ;
#4080 = VERTEX_POINT ( 'NONE', #10986 ) ;
#4081 = CARTESIAN_POINT ( 'NONE',  ( -4.243569643749997233, -18.04319075220617563, -5.758356952251413752 ) ) ;
#4082 = CARTESIAN_POINT ( 'NONE',  ( 2.211161402132902243, 19.62180007765647360, 2.942372952327172442 ) ) ;
#4083 = SURFACE_STYLE_FILL_AREA ( #14096 ) ;
#4084 = CARTESIAN_POINT ( 'NONE',  ( -5.330712181944246111E-15, -26.26870678593456887, -4.691140945321855327 ) ) ;
#4085 = EDGE_CURVE ( 'NONE', #9743, #1083, #9593, .T. ) ;
#4086 = DIRECTION ( 'NONE',  ( 0.000000000000000000, -0.4999999999999990563, 0.8660254037844391517 ) ) ;
#4087 = AXIS2_PLACEMENT_3D ( 'NONE', #5491, #11314, #13932 ) ;
#4088 = CARTESIAN_POINT ( 'NONE',  ( -3.706921591972381904E-14, -17.67153205169451624, -7.929870390770359379 ) ) ;
#4089 = LINE ( 'NONE', #7133, #14774 ) ;
#4090 = CIRCLE ( 'NONE', #3215, 0.9999999999999991118 ) ;
#4091 = ORIENTED_EDGE ( 'NONE', *, *, #11924, .F. ) ;
#4092 = AXIS2_PLACEMENT_3D ( 'NONE', #8633, #15701, #13093 ) ;
#4093 = VERTEX_POINT ( 'NONE', #6450 ) ;
#4094 = CARTESIAN_POINT ( 'NONE',  ( -2.798362969681365886, 25.24680007765647716, 2.102939460078824929 ) ) ;
#4095 = EDGE_CURVE ( 'NONE', #10626, #13628, #16694, .T. ) ;
#4096 = CARTESIAN_POINT ( 'NONE',  ( -5.577813053751546416E-15, -25.19265864305380376, -4.723577975706471754 ) ) ;
#4097 = CARTESIAN_POINT ( 'NONE',  ( -9.000000000000001776, 25.39999999999999503, 2.499999999999995559 ) ) ;
#4098 = DIRECTION ( 'NONE',  ( -0.000000000000000000, -0.5735764363510414965, -0.8191520442889950182 ) ) ;
#4099 = ORIENTED_EDGE ( 'NONE', *, *, #15232, .F. ) ;
#4100 = CARTESIAN_POINT ( 'NONE',  ( -2.500000000000001332, 34.50319992234354771, -0.05647727720530596601 ) ) ;
#4101 = CARTESIAN_POINT ( 'NONE',  ( 4.730628863548789710E-15, -20.17675178328056873, -13.07688799768438948 ) ) ;
#4102 = CARTESIAN_POINT ( 'NONE',  ( 2.211161402132902243, 32.12180007765647360, 2.942372952327172442 ) ) ;
#4103 = CARTESIAN_POINT ( 'NONE',  ( -2.115076519116425580, 24.87819992234354771, -3.012182706137062738 ) ) ;
#4104 = LINE ( 'NONE', #12809, #1065 ) ;
#4105 = DIRECTION ( 'NONE',  ( 0.000000000000000000, 0.8191520442889952403, -0.5735764363510413855 ) ) ;
#4106 = MECHANICAL_DESIGN_GEOMETRIC_PRESENTATION_REPRESENTATION (  '', ( #5592 ), #4682 ) ;
#4107 = CARTESIAN_POINT ( 'NONE',  ( 4.730628863548789710E-15, -19.95090606146734658, -12.75434688024559726 ) ) ;
#4108 = VECTOR ( 'NONE', #14757, 1000.000000000000000 ) ;
#4109 = VECTOR ( 'NONE', #6956, 1000.000000000000000 ) ;
#4110 =( BOUNDED_CURVE ( )  B_SPLINE_CURVE ( 2, ( #14202, #18309, #5581, #16915, #9923, #6786, #12713, #8273, #4192 ),
 .UNSPECIFIED., .F., .T. ) 
 B_SPLINE_CURVE_WITH_KNOTS ( ( 3, 2, 2, 2, 3 ),
 ( 0.5431034482758620996, 0.5459770114942529284, 0.5517241379310344751, 0.5574712643678161328, 0.5603448275862069616 ),
 .UNSPECIFIED. ) 
 CURVE ( )  GEOMETRIC_REPRESENTATION_ITEM ( )  RATIONAL_B_SPLINE_CURVE ( ( 0.9330127018922194093, 0.9330127018922194093, 1.000000000000000000, 0.8660254037844387076, 1.000000000000000000, 0.8660254037844387076, 1.000000000000000000, 0.9330127018922180770, 0.9330127018922194093 ) ) 
 REPRESENTATION_ITEM ( '' )  );
#4111 = CARTESIAN_POINT ( 'NONE',  ( 9.000000000000000000, 18.79999999999999361, -2.500000000000001332 ) ) ;
#4112 = ADVANCED_FACE ( 'NONE', ( #16756 ), #12190, .T. ) ;
#4113 = EDGE_CURVE ( 'NONE', #9296, #12103, #2559, .T. ) ;
#4114 = DIRECTION ( 'NONE',  ( -0.000000000000000000, -0.5735764363510414965, -0.8191520442889950182 ) ) ;
#4115 = ADVANCED_FACE ( 'NONE', ( #2386 ), #990, .T. ) ;
#4116 = DIRECTION ( 'NONE',  ( 0.000000000000000000, 0.000000000000000000, 1.000000000000000000 ) ) ;
#4117 = CARTESIAN_POINT ( 'NONE',  ( -4.243569643750000786, -21.80312760463873900, -6.856613161887861629 ) ) ;
#4118 = CYLINDRICAL_SURFACE ( 'NONE', #11509, 4.000000000000000000 ) ;
#4119 = FACE_BOUND ( 'NONE', #9018, .T. ) ;
#4120 = VECTOR ( 'NONE', #8235, 1000.000000000000000 ) ;
#4121 = CARTESIAN_POINT ( 'NONE',  ( -0.8262555684461330152, 35.99680007765648071, -2.360188852285403982 ) ) ;
#4122 = VECTOR ( 'NONE', #16053, 1000.000000000000000 ) ;
#4123 = CARTESIAN_POINT ( 'NONE',  ( 4.299564228933482956E-15, -19.22018842984233089, -10.14158091035064579 ) ) ;
#4124 = CARTESIAN_POINT ( 'NONE',  ( 2.864755990943265829, 36.99680007765648071, 2.011557305968487697 ) ) ;
#4125 = CARTESIAN_POINT ( 'NONE',  ( -5.577813053751546416E-15, -29.06429958842333505, -10.25285427465718868 ) ) ;
#4126 = DIRECTION ( 'NONE',  ( 0.000000000000000000, 0.000000000000000000, 1.000000000000000000 ) ) ;
#4127 = ORIENTED_EDGE ( 'NONE', *, *, #2592, .T. ) ;
#4129 = CARTESIAN_POINT ( 'NONE',  ( 4.730628863548789710E-15, -17.88603089060359963, -9.805399520805213598 ) ) ;
#4128 = CIRCLE ( 'NONE', #16880, 0.9999999999999991118 ) ;
#4130 = CARTESIAN_POINT ( 'NONE',  ( 3.481649420246369697, 34.12180007765648071, -1.193696214020541824 ) ) ;
#4131 = CIRCLE ( 'NONE', #12999, 8.000000000000000000 ) ;
#4132 = AXIS2_PLACEMENT_3D ( 'NONE', #18368, #4249, #18101 ) ;
#4133 = DIRECTION ( 'NONE',  ( -0.000000000000000000, -1.000000000000000000, -0.000000000000000000 ) ) ;
#4134 = DIRECTION ( 'NONE',  ( -0.000000000000000000, -1.000000000000000000, -0.000000000000000000 ) ) ;
#4135 = CARTESIAN_POINT ( 'NONE',  ( 13.00000000000000178, 15.00000000000000178, 16.00000000000000000 ) ) ;
#4136 = DIRECTION ( 'NONE',  ( 0.7601375407242620952, 0.6497622020259954390, 0.000000000000000000 ) ) ;
#4137 = CARTESIAN_POINT ( 'NONE',  ( -4.243569643750000786, -26.44909673908217584, -13.49174472062871999 ) ) ;
#4138 = ORIENTED_EDGE ( 'NONE', *, *, #15552, .F. ) ;
#4139 = CARTESIAN_POINT ( 'NONE',  ( -1.661723472263481630E-14, -20.25262601527420969, -11.61605459007084029 ) ) ;
#4140 = CARTESIAN_POINT ( 'NONE',  ( 2.000000000000004441, -18.97087896441710697, -8.851219772375051420 ) ) ;
#4141 = CARTESIAN_POINT ( 'NONE',  ( 2.481649420246374138, 16.62180007765648071, -0.8687765177876252132 ) ) ;
#4142 = EDGE_LOOP ( 'NONE', ( #14105, #3638, #12025, #940 ) ) ;
#4143 = CARTESIAN_POINT ( 'NONE',  ( 0.000000000000000000, 1.443375672974065216, 7.222237291452134449E-31 ) ) ;
#4144 = EDGE_CURVE ( 'NONE', #17585, #6078, #11324, .T. ) ;
#4145 = FILL_AREA_STYLE_COLOUR ( '', #1260 ) ;
#4146 = AXIS2_PLACEMENT_3D ( 'NONE', #4677, #2105, #7733 ) ;
#4147 = CARTESIAN_POINT ( 'NONE',  ( -3.607379964056306676, 17.74680007765647716, 2.690724712371306282 ) ) ;
#4148 = DIRECTION ( 'NONE',  ( -1.000000000000000000, -0.000000000000000000, -0.000000000000000000 ) ) ;
#4149 = CARTESIAN_POINT ( 'NONE',  ( -3.500000000000000444, 14.50319992234354416, -0.05647727720529563400 ) ) ;
#4150 = EDGE_LOOP ( 'NONE', ( #13636, #4005, #4634, #13466 ) ) ;
#4151 = CARTESIAN_POINT ( 'NONE',  ( -2.121784821874996396, -22.73963465402730577, -14.60131900523419901 ) ) ;
#4152 = CARTESIAN_POINT ( 'NONE',  ( 2.829195390882805583, 34.62180007765646650, 3.793023760679204770 ) ) ;
#4153 = ORIENTED_EDGE ( 'NONE', *, *, #10556, .F. ) ;
#4154 = CYLINDRICAL_SURFACE ( 'NONE', #288, 4.000000000000000000 ) ;
#4155 = CARTESIAN_POINT ( 'NONE',  ( -8.000000000000001776, 20.99999999999999289, 2.499999999999998224 ) ) ;
#4156 = CARTESIAN_POINT ( 'NONE',  ( 0.000000000000000000, 46.00000000000000000, 2.500000000000000000 ) ) ;
#4157 = AXIS2_PLACEMENT_3D ( 'NONE', #16906, #11305, #4182 ) ;
#4158 = CARTESIAN_POINT ( 'NONE',  ( 0.000000000000000000, 15.00000000000000355, 5.000000000000000000 ) ) ;
#4159 = CARTESIAN_POINT ( 'NONE',  ( -4.243569643750005227, -24.59515422072892221, -6.572550296786629609 ) ) ;
#4160 = EDGE_CURVE ( 'NONE', #9997, #1782, #12097, .T. ) ;
#4161 = VERTEX_POINT ( 'NONE', #9319 ) ;
#4162 = APPLICATION_CONTEXT ( 'automotive_design' ) ;
#4163 = LINE ( 'NONE', #12318, #2355 ) ;
#4164 = ADVANCED_FACE ( 'NONE', ( #10892 ), #14612, .T. ) ;
#4165 = VERTEX_POINT ( 'NONE', #2478 ) ;
#4166 = CARTESIAN_POINT ( 'NONE',  ( -4.000000000000004441, -26.43191327531376800, -9.440886284020393759 ) ) ;
#4167 = CARTESIAN_POINT ( 'NONE',  ( 0.000000000000000000, -0.7216878364870317197, -1.250000000000000000 ) ) ;
#4168 = EDGE_CURVE ( 'NONE', #16215, #3649, #17597, .T. ) ;
#4169 = CARTESIAN_POINT ( 'NONE',  ( -10.00000000000000178, 34.19999999999999574, -2.500000000000001776 ) ) ;
#4170 = CARTESIAN_POINT ( 'NONE',  ( -1.336863392178569088, 17.50319992234354771, -4.297206761780648421 ) ) ;
#4171 = CARTESIAN_POINT ( 'NONE',  ( -1.135272562821019626, 19.00319992234354771, 3.311245368580577164 ) ) ;
#4172 = CARTESIAN_POINT ( 'NONE',  ( 4.713407268011036227E-15, -21.87513548686850129, -15.01208688952113057 ) ) ;
#4173 = CARTESIAN_POINT ( 'NONE',  ( 1.593127413382998903, 34.62180007765648071, 2.091722143975139669 ) ) ;
#4174 = AXIS2_PLACEMENT_3D ( 'NONE', #13691, #5620, #9786 ) ;
#4175 = CARTESIAN_POINT ( 'NONE',  ( 4.518350579753602325, 23.12819992234354416, -1.405661355842793725 ) ) ;
#4176 = CARTESIAN_POINT ( 'NONE',  ( -2.000000000000005773, -26.51742392663723180, -7.549849196723933176 ) ) ;
#4177 = EDGE_LOOP ( 'NONE', ( #11943, #1017, #253, #9566 ) ) ;
#4178 = LINE ( 'NONE', #17267, #15953 ) ;
#4179 = CARTESIAN_POINT ( 'NONE',  ( -2.211161402132902243, 23.37180007765647716, -2.942372952327172886 ) ) ;
#4180 = CARTESIAN_POINT ( 'NONE',  ( 2.121784821874994176, -26.01805392422797070, -6.468916616312057499 ) ) ;
#4181 = COLOUR_RGB ( '',0.8941176470588234615, 0.8941176470588234615, 0.8941176470588234615 ) ;
#4182 = DIRECTION ( 'NONE',  ( 0.000000000000000000, 0.000000000000000000, -1.000000000000000000 ) ) ;
#4183 = CARTESIAN_POINT ( 'NONE',  ( 0.000000000000000000, 9.254131787996968228, 30.52396275209373044 ) ) ;
#4184 = DIRECTION ( 'NONE',  ( -0.000000000000000000, -0.000000000000000000, 1.000000000000000000 ) ) ;
#4185 = ADVANCED_FACE ( 'NONE', ( #1080 ), #16665, .F. ) ;
#4186 = ORIENTED_EDGE ( 'NONE', *, *, #7385, .T. ) ;
#4187 = ORIENTED_EDGE ( 'NONE', *, *, #3565, .F. ) ;
#4188 = CARTESIAN_POINT ( 'NONE',  ( -1.135272562821090014, 20.99680007765647716, -3.311245368580554072 ) ) ;
#4189 = FACE_OUTER_BOUND ( 'NONE', #11845, .T. ) ;
#4190 = CARTESIAN_POINT ( 'NONE',  ( -1.071796769724486786, -22.88672062792949546, -15.37793156070467582 ) ) ;
#4191 = CARTESIAN_POINT ( 'NONE',  ( 4.000000000000003553, -19.16393519826133485, -7.113773694389544211 ) ) ;
#4192 = CARTESIAN_POINT ( 'NONE',  ( -3.706921591972381904E-14, -19.54282517599473579, -10.60235393626997080 ) ) ;
#4193 = ORIENTED_EDGE ( 'NONE', *, *, #17852, .F. ) ;
#4194 = CARTESIAN_POINT ( 'NONE',  ( 3.518350579753605434, 15.62819992234354416, -1.080741659609877114 ) ) ;
#4195 = CARTESIAN_POINT ( 'NONE',  ( 4.243569643750003451, -20.93616690305174544, -9.889955075634029313 ) ) ;
#4196 = CARTESIAN_POINT ( 'NONE',  ( -2.864755990943265829, 33.24680007765648071, -2.011557305968488141 ) ) ;
#4197 = CARTESIAN_POINT ( 'NONE',  ( -0.05938372350920063936, 26.37819992234354061, 3.680117784833935701 ) ) ;
#4198 = CARTESIAN_POINT ( 'NONE',  ( 1.300000000000000044, -1.082531754730548412, -0.6250000000000003331 ) ) ;
#4199 = LINE ( 'NONE', #17100, #2276 ) ;
#4200 = MECHANICAL_DESIGN_GEOMETRIC_PRESENTATION_REPRESENTATION (  '', ( #2717 ), #13665 ) ;
#4201 = CARTESIAN_POINT ( 'NONE',  ( 4.243569643750003451, -22.25897755938633793, -11.77912447777552352 ) ) ;
#4202 = CARTESIAN_POINT ( 'NONE',  ( -0.3217809247881409651, -15.45745613286858422, -10.86990606519723279 ) ) ;
#4203 = VECTOR ( 'NONE', #11705, 999.9999999999998863 ) ;
#4204 = CARTESIAN_POINT ( 'NONE',  ( -9.000000000000001776, 43.00000000000000000, 2.499999999999995559 ) ) ;
#4205 = AXIS2_PLACEMENT_3D ( 'NONE', #10570, #17468, #10288 ) ;
#4206 = LINE ( 'NONE', #11149, #15935 ) ;
#4207 = CARTESIAN_POINT ( 'NONE',  ( -4.243569643749997233, -18.01092707766142809, -5.712279649760157341 ) ) ;
#4208 = DIRECTION ( 'NONE',  ( 0.000000000000000000, 0.8191520442889952403, -0.5735764363510413855 ) ) ;
#4209 = ORIENTED_EDGE ( 'NONE', *, *, #13852, .T. ) ;
#4210 = CARTESIAN_POINT ( 'NONE',  ( 2.500000000000001332, 39.24680007765647360, -0.05647727720535888202 ) ) ;
#4211 = CARTESIAN_POINT ( 'NONE',  ( 2.121784821874994176, -29.37347607688156259, -11.26095607540267807 ) ) ;
#4212 = CARTESIAN_POINT ( 'NONE',  ( 3.518350579753631191, 39.37180007765646650, 1.080741659609802729 ) ) ;
#4213 = CONTEXT_DEPENDENT_SHAPE_REPRESENTATION ( #9844, #12079 ) ;
#4214 = DIRECTION ( 'NONE',  ( 0.000000000000000000, 0.000000000000000000, 1.000000000000000000 ) ) ;
#4215 = EDGE_CURVE ( 'NONE', #8977, #11296, #11590, .T. ) ;
#4216 = ORIENTED_EDGE ( 'NONE', *, *, #17333, .F. ) ;
#4217 = AXIS2_PLACEMENT_3D ( 'NONE', #16498, #3872, #2316 ) ;
#4218 = CARTESIAN_POINT ( 'NONE',  ( -5.330712181944246111E-15, -23.71987649689963362, -1.051034048512634156 ) ) ;
#4219 = CARTESIAN_POINT ( 'NONE',  ( 1.135272562821090458, 34.74680007765648071, 3.311245368580554072 ) ) ;
#4220 = VECTOR ( 'NONE', #4530, 1000.000000000000000 ) ;
#4221 = EDGE_CURVE ( 'NONE', #17692, #5913, #3356, .T. ) ;
#4222 =( BOUNDED_CURVE ( )  B_SPLINE_CURVE ( 2, ( #14259, #2951, #6086, #1751, #7475, #10349, #8584, #7198, #17341 ),
 .UNSPECIFIED., .F., .F. ) 
 B_SPLINE_CURVE_WITH_KNOTS ( ( 3, 2, 2, 2, 3 ),
 ( 0.5948275862068965747, 0.5977011494252874035, 0.6034482758620689502, 0.6091954022988506079, 0.6120689655172414367 ),
 .UNSPECIFIED. ) 
 CURVE ( )  GEOMETRIC_REPRESENTATION_ITEM ( )  RATIONAL_B_SPLINE_CURVE ( ( 0.9330127018922194093, 0.9330127018922194093, 1.000000000000000000, 0.8660254037844387076, 1.000000000000000000, 0.8660254037844387076, 1.000000000000000000, 0.9330127018922180770, 0.9330127018922194093 ) ) 
 REPRESENTATION_ITEM ( '' )  );
#4223 = EDGE_CURVE ( 'NONE', #5777, #9873, #9773, .T. ) ;
#4224 = CARTESIAN_POINT ( 'NONE',  ( 8.500000000000019540, 0.000000000000000000, 20.49999999999998934 ) ) ;
#4225 = CARTESIAN_POINT ( 'NONE',  ( 13.00000000000000178, 49.00000000000000000, 16.00000000000000000 ) ) ;
#4226 = EDGE_CURVE ( 'NONE', #8512, #5725, #7478, .T. ) ;
#4227 = CARTESIAN_POINT ( 'NONE',  ( -8.999999999999996447, -4.000000000000000000, 30.00000000000000000 ) ) ;
#4228 = FACE_OUTER_BOUND ( 'NONE', #7273, .T. ) ;
#4229 = CARTESIAN_POINT ( 'NONE',  ( -4.243569643750005227, -26.88587511340589131, -9.844038773665802822 ) ) ;
#4230 = ORIENTED_EDGE ( 'NONE', *, *, #1117, .F. ) ;
#4231 = CYLINDRICAL_SURFACE ( 'NONE', #12756, 4.000000000000001776 ) ;
#4232 = AXIS2_PLACEMENT_3D ( 'NONE', #5196, #9187, #14773 ) ;
#4233 = CARTESIAN_POINT ( 'NONE',  ( 2.000000000000004441, -18.19655077534320498, -7.745364512584909988 ) ) ;
#4234 = PRESENTATION_LAYER_ASSIGNMENT (  '', '', ( #1885 ) ) ;
#4235 = CARTESIAN_POINT ( 'NONE',  ( 0.05938372350927906274, 39.87180007765648071, 3.680117784833935701 ) ) ;
#4236 = EDGE_LOOP ( 'NONE', ( #11681, #1803 ) ) ;
#4237 = EDGE_CURVE ( 'NONE', #4992, #6649, #3172, .T. ) ;
#4238 = CARTESIAN_POINT ( 'NONE',  ( -1.734723475976807094E-15, 23.19999999999999574, -2.500000000000000000 ) ) ;
#4239 = CARTESIAN_POINT ( 'NONE',  ( 2.199999999999999734, 0.000000000000000000, 2.200000000000000178 ) ) ;
#4240 = CARTESIAN_POINT ( 'NONE',  ( -1.593127413382952939, 36.62819992234354771, 2.091722143975172532 ) ) ;
#4241 = PRODUCT_RELATED_PRODUCT_CATEGORY ( 'part', '', ( #9448 ) ) ;
#4242 = ORIENTED_EDGE ( 'NONE', *, *, #6216, .F. ) ;
#4243 = CARTESIAN_POINT ( 'NONE',  ( 4.243569643750003451, -23.29141514481821318, -13.25359815749571268 ) ) ;
#4244 = CARTESIAN_POINT ( 'NONE',  ( 2.829195390882805583, 32.12180007765646650, 3.793023760679204770 ) ) ;
#4245 = EDGE_LOOP ( 'NONE', ( #5453, #9525, #15281, #3672 ) ) ;
#4246 = VECTOR ( 'NONE', #4876, 1000.000000000000000 ) ;
#4247 = FACE_OUTER_BOUND ( 'NONE', #14267, .T. ) ;
#4248 = CARTESIAN_POINT ( 'NONE',  ( 4.000000000000000000, -1.759474945355381292, 3.047500000000002540 ) ) ;
#4249 = DIRECTION ( 'NONE',  ( 0.000000000000000000, 0.000000000000000000, 1.000000000000000000 ) ) ;
#4250 = CARTESIAN_POINT ( 'NONE',  ( 4.243569643750003451, -20.71032118123852683, -9.567413958195238877 ) ) ;
#4251 = ORIENTED_EDGE ( 'NONE', *, *, #5422, .F. ) ;
#4252 = CARTESIAN_POINT ( 'NONE',  ( -9.000000000000001776, 40.79999999999999716, 2.499999999999998224 ) ) ;
#4253 = VERTEX_POINT ( 'NONE', #15974 ) ;
#4254 = CARTESIAN_POINT ( 'NONE',  ( 1.999999999999994449, -27.57137062913722048, -9.055041079111724400 ) ) ;
#4255 = CYLINDRICAL_SURFACE ( 'NONE', #9534, 4.000000000000000888 ) ;
#4256 = TOROIDAL_SURFACE ( 'NONE', #14941, 9.000000000000003553, 0.9999999999999991118 ) ;
#4257 = DIRECTION ( 'NONE',  ( -0.000000000000000000, 1.000000000000000000, -0.000000000000000000 ) ) ;
#4258 =( NAMED_UNIT ( * ) SI_UNIT ( $, .STERADIAN. ) SOLID_ANGLE_UNIT ( ) );
#4259 = CARTESIAN_POINT ( 'NONE',  ( 0.05938372350919016857, 15.12819992234354594, -4.731580009072201776 ) ) ;
#4260 = CARTESIAN_POINT ( 'NONE',  ( -2.211161402132838738, 24.12819992234354416, 2.942372952327218183 ) ) ;
#4261 = CARTESIAN_POINT ( 'NONE',  ( -2.000000000000005773, -28.90493584365338720, -10.95956958208364007 ) ) ;
#4262 = CARTESIAN_POINT ( 'NONE',  ( -2.481649420246391902, 14.62819992234354594, -0.8687765177875723666 ) ) ;
#4263 = CARTESIAN_POINT ( 'NONE',  ( 4.481649420246397675, 30.87819992234354061, 1.518615910253363177 ) ) ;
#4264 = TOROIDAL_SURFACE ( 'NONE', #16745, 9.000000000000001776, 0.9999999999999991118 ) ;
#4265 = CARTESIAN_POINT ( 'NONE',  ( 3.999999999999996447, -25.76513066735074986, -8.488622031527665257 ) ) ;
#4266 = ORIENTED_EDGE ( 'NONE', *, *, #2242, .F. ) ;
#4267 = DIRECTION ( 'NONE',  ( 0.000000000000000000, 0.000000000000000000, 1.000000000000000000 ) ) ;
#4268 = CARTESIAN_POINT ( 'NONE',  ( -3.500000000000000444, 25.49680007765647716, 0.05647727720536892260 ) ) ;
#4269 = CARTESIAN_POINT ( 'NONE',  ( 9.993653656444104527, -9.917152142463184106, 4.126537876780505876 ) ) ;
#4270 = CARTESIAN_POINT ( 'NONE',  ( 4.243569643750000786, -22.70651049189163828, -8.146777631643026041 ) ) ;
#4271 = CARTESIAN_POINT ( 'NONE',  ( 4.481649420246366589, 21.62180007765647716, -1.518615910253458212 ) ) ;
#4272 = CARTESIAN_POINT ( 'NONE',  ( -1.999999999999996225, -17.12109495718499375, -6.209454429543042941 ) ) ;
#4273 = CARTESIAN_POINT ( 'NONE',  ( 3.579096709490575479E-14, -26.48320562484364871, -6.566670075356708658 ) ) ;
#4274 = ORIENTED_EDGE ( 'NONE', *, *, #10452, .F. ) ;
#4275 = ORIENTED_EDGE ( 'NONE', *, *, #13245, .F. ) ;
#4276 = CARTESIAN_POINT ( 'NONE',  ( -1.027846397803541700, 22.49680007765648071, 3.346150245485522312 ) ) ;
#4277 = DIRECTION ( 'NONE',  ( -0.000000000000000000, -1.000000000000000000, -0.000000000000000000 ) ) ;
#4278 = SURFACE_SIDE_STYLE ('',( #9921 ) ) ;
#4279 = CARTESIAN_POINT ( 'NONE',  ( 3.579096709490575479E-14, -24.41833045397989821, -3.617722715916328546 ) ) ;
#4280 = DIRECTION ( 'NONE',  ( 0.000000000000000000, 0.000000000000000000, 1.000000000000000000 ) ) ;
#4281 = VERTEX_POINT ( 'NONE', #6126 ) ;
#4282 = CARTESIAN_POINT ( 'NONE',  ( -2.798362969681409851, 22.25319992234354416, -2.102939460078765421 ) ) ;
#4283 = CARTESIAN_POINT ( 'NONE',  ( -2.121784821874996396, -20.38438641226084158, -11.23767592337251209 ) ) ;
#4284 = CARTESIAN_POINT ( 'NONE',  ( 0.05938372350927906274, 39.87180007765648071, 3.680117784833935701 ) ) ;
#4285 = CARTESIAN_POINT ( 'NONE',  ( -0.05938372350920063936, 33.87819992234354771, 3.680117784833935701 ) ) ;
#4286 = LINE ( 'NONE', #9931, #160 ) ;
#4287 = CARTESIAN_POINT ( 'NONE',  ( -8.999999999999996447, -4.000000000000000000, -30.00000000000000000 ) ) ;
#4288 = CARTESIAN_POINT ( 'NONE',  ( -2.121784821875005722, -25.06089824606716476, -5.101956642404802622 ) ) ;
#4289 = EDGE_CURVE ( 'NONE', #7899, #1548, #16098, .T. ) ;
#4290 = DIRECTION ( 'NONE',  ( 0.000000000000000000, 0.000000000000000000, 1.000000000000000000 ) ) ;
#4291 = FACE_OUTER_BOUND ( 'NONE', #14344, .T. ) ;
#4292 = CYLINDRICAL_SURFACE ( 'NONE', #10302, 2.000000000000001776 ) ;
#4293 = CARTESIAN_POINT ( 'NONE',  ( -4.243569643750005227, -22.23990597896245447, -3.208907214924944462 ) ) ;
#4294 = CARTESIAN_POINT ( 'NONE',  ( 1.820000000000000062, 0.000000000000000000, 0.000000000000000000 ) ) ;
#4295 = CARTESIAN_POINT ( 'NONE',  ( -13.00000000000000178, 49.00000000000000000, 16.00000000000000000 ) ) ;
#4296 = ORIENTED_EDGE ( 'NONE', *, *, #15457, .F. ) ;
#4297 = CARTESIAN_POINT ( 'NONE',  ( 0.8262555684460829442, 22.75319992234354771, -2.360188852285421302 ) ) ;
#4298 = CARTESIAN_POINT ( 'NONE',  ( 4.243569643750003451, -24.29158905570534088, -14.68199453472465166 ) ) ;
#4299 = CARTESIAN_POINT ( 'NONE',  ( 0.05938372350927906274, 17.37180007765647005, 3.680117784833935701 ) ) ;
#4300 = FACE_OUTER_BOUND ( 'NONE', #6390, .T. ) ;
#4301 = FACE_OUTER_BOUND ( 'NONE', #961, .T. ) ;
#4302 = ORIENTED_EDGE ( 'NONE', *, *, #2083, .F. ) ;
#4303 = CARTESIAN_POINT ( 'NONE',  ( 2.121784821874994176, -23.46922363519303190, -2.828809719502837439 ) ) ;
#4304 = CARTESIAN_POINT ( 'NONE',  ( 3.518350579753631191, 34.37180007765648071, 1.080741659609802285 ) ) ;
#4305 = CARTESIAN_POINT ( 'NONE',  ( 1.300000000000000044, -1.443375672974064328, 1.278502688459867223E-18 ) ) ;
#4306 = CARTESIAN_POINT ( 'NONE',  ( -5.330712181944246111E-15, -29.36601954223019462, -9.114561984482429935 ) ) ;
#4307 = CARTESIAN_POINT ( 'NONE',  ( -8.000000000000001776, 40.79999999999999716, 2.499999999999998224 ) ) ;
#4308 = CARTESIAN_POINT ( 'NONE',  ( -3.706921591972381904E-14, -18.25227819420489439, -8.759261836619732122 ) ) ;
#4309 = DIRECTION ( 'NONE',  ( -0.000000000000000000, -0.5735764363510414965, -0.8191520442889950182 ) ) ;
#4310 = CIRCLE ( 'NONE', #14706, 0.9999999999999991118 ) ;
#4311 = CARTESIAN_POINT ( 'NONE',  ( 4.730628863548789710E-15, -21.20918936871244043, -14.55136167740457864 ) ) ;
#4312 = EDGE_CURVE ( 'NONE', #6560, #8602, #13107, .T. ) ;
#4313 = CARTESIAN_POINT ( 'NONE',  ( -3.999999999999997335, -21.85257474295189084, -10.95354890098744605 ) ) ;
#4314 = CARTESIAN_POINT ( 'NONE',  ( -4.000000000000004441, -22.81838172630220996, -4.280228404999725456 ) ) ;
#4315 = CARTESIAN_POINT ( 'NONE',  ( 0.8262555684461332373, 19.74680007765648071, 2.360188852285403982 ) ) ;
#4316 = EDGE_CURVE ( 'NONE', #12374, #5212, #13708, .T. ) ;
#4317 = ORIENTED_EDGE ( 'NONE', *, *, #8030, .F. ) ;
#4318 = CARTESIAN_POINT ( 'NONE',  ( 9.000000000000000000, 43.00000000000000000, -2.500000000000001332 ) ) ;
#4319 = SURFACE_STYLE_USAGE ( .BOTH. , #7095 ) ;
#4320 = CARTESIAN_POINT ( 'NONE',  ( -4.000000000000004441, -24.88325689716596045, -7.229175764440105567 ) ) ;
#4321 = CARTESIAN_POINT ( 'NONE',  ( 1.989345975306457071, 38.50319992234354771, 1.515154207786300500 ) ) ;
#4322 =( BOUNDED_CURVE ( )  B_SPLINE_CURVE ( 2, ( #3451, #17836, #13361, #9364, #15040, #13630, #6586, #7700, #11969, #17661, #16249, #5381, #18205, #9457, #12420, #1397, #5469, #3986, #5557, #11114, #13911, #2792, #14085, #11205, #7025, #5648, #6762, #8154, #15130, #16894, #12510, #2612, #2434, #2705, #4171, #16803, #8060, #13723, #18014, #16713, #5286, #18111, #4073, #3899, #9635, #8337, #15224, #9725, #973, #10941, #1219, #3802, #9814, #1034, #11030, #15313, #15410, #8252, #18284, #6856, #13996, #1311, #12689, #15495, #8423, #11291, #6943, #6674, #12596, #12328, #16624, #9546, #2524, #13816, #1127, #4260, #4532, #9903, #6008, #3245, #2875, #461, #14365, #12779, #6102, #4438, #2963, #8688, #1664, #7300, #369, #14178, #12960, #8597, #14464, #174, #275, #15574, #7213, #14561, #5919, #88, #13150, #3057, #10174, #15948, #8883, #11663, #1861, #16983, #1575, #14272, #8505, #17355, #11564, #15757, #1485, #15851, #4618, #17259, #7119, #3149, #7492, #13058, #4343, #12867, #8783, #17068, #10078, #1767, #9990, #7398, #5741, #11381, #10268, #15665, #5825, #11470, #17164, #14750, #4990, #651, #3430, #11850, #10646, #6295, #3695, #6471, #16411, #9341, #10549, #3604, #17546, #9254, #9071, #10737, #16225, #16318, #14939, #12031, #13607, #2231, #12123, #2319, #3518, #11948, #7677, #15019, #17448, #830, #1957, #7950, #9165, #4716, #14846, #14657, #8984, #7583, #921, #6388, #17817, #559, #5078, #7857, #13241, #10367, #16046, #10463, #6201, #3338, #4815, #11754, #13430, #17642, #13514, #744, #2139, #17724, #7770 ),
 .UNSPECIFIED., .F., .F. ) 
 B_SPLINE_CURVE_WITH_KNOTS ( ( 3, 2, 2, 2, 2, 2, 2, 2, 2, 2, 2, 2, 2, 2, 2, 2, 2, 2, 2, 2, 2, 2, 2, 2, 2, 2, 2, 2, 2, 2, 2, 2, 2, 2, 2, 2, 2, 2, 2, 2, 2, 2, 2, 2, 2, 2, 2, 2, 2, 2, 2, 2, 2, 2, 2, 2, 2, 2, 2, 2, 2, 2, 2, 2, 2, 2, 2, 2, 2, 2, 2, 2, 2, 2, 2, 2, 2, 2, 2, 2, 2, 2, 2, 2, 2, 2, 2, 2, 2, 2, 2, 2, 2, 2, 2, 2, 2, 2, 2, 3 ),
 ( 0.01986568351594109050, 0.02000000000000000042, 0.02999999999999999889, 0.04000000000000000083, 0.05000000000000000278, 0.05999999999999999778, 0.07000000000000000666, 0.08000000000000000167, 0.08999999999999999667, 0.1000000000000000056, 0.1100000000000000006, 0.1199999999999999956, 0.1300000000000000044, 0.1400000000000000133, 0.1499999999999999944, 0.1600000000000000033, 0.1699999999999999845, 0.1799999999999999933, 0.1900000000000000022, 0.2000000000000000111, 0.2099999999999999922, 0.2200000000000000289, 0.2300000000000000100, 0.2399999999999999911, 0.2500000000000000000, 0.2600000000000000089, 0.2700000000000000178, 0.2800000000000000266, 0.2899999999999999800, 0.2999999999999999889, 0.3099999999999999978, 0.3200000000000000067, 0.3300000000000000155, 0.3400000000000000244, 0.3499999999999999778, 0.3599999999999999867, 0.3699999999999999956, 0.3800000000000000044, 0.3900000000000000133, 0.4000000000000000222, 0.4099999999999999756, 0.4199999999999999845, 0.4299999999999999933, 0.4400000000000000022, 0.4500000000000000111, 0.4600000000000000200, 0.4699999999999999734, 0.4799999999999999822, 0.4899999999999999911, 0.5000000000000000000, 0.5100000000000000089, 0.5200000000000000178, 0.5300000000000000266, 0.5400000000000000355, 0.5500000000000000444, 0.5600000000000000533, 0.5699999999999999512, 0.5799999999999999600, 0.5899999999999999689, 0.5999999999999999778, 0.6099999999999999867, 0.6199999999999999956, 0.6300000000000000044, 0.6400000000000000133, 0.6500000000000000222, 0.6600000000000000311, 0.6700000000000000400, 0.6800000000000000488, 0.6899999999999999467, 0.6999999999999999556, 0.7099999999999999645, 0.7199999999999999734, 0.7299999999999999822, 0.7399999999999999911, 0.7500000000000000000, 0.7600000000000000089, 0.7700000000000000178, 0.7800000000000000266, 0.7900000000000000355, 0.8000000000000000444, 0.8100000000000000533, 0.8199999999999999512, 0.8299999999999999600, 0.8399999999999999689, 0.8499999999999999778, 0.8599999999999999867, 0.8699999999999999956, 0.8800000000000000044, 0.8900000000000000133, 0.9000000000000000222, 0.9100000000000000311, 0.9200000000000000400, 0.9300000000000000488, 0.9399999999999999467, 0.9499999999999999556, 0.9599999999999999645, 0.9699999999999999734, 0.9799999999999999822, 0.9899999999999999911, 1.000000000000000000 ),
 .UNSPECIFIED. ) 
 CURVE ( )  GEOMETRIC_REPRESENTATION_ITEM ( )  RATIONAL_B_SPLINE_CURVE ( ( 0.9987028763776494289, 0.9993426083351170108, 1.000000000000000000, 0.9510565162951535312, 1.000000000000000000, 0.9510565162951535312, 1.000000000000000000, 0.9510565162951535312, 1.000000000000000000, 0.9510565162951535312, 1.000000000000000000, 0.9510565162951535312, 1.000000000000000000, 0.9510565162951535312, 1.000000000000000000, 0.9510565162951535312, 1.000000000000000000, 0.9510565162951535312, 1.000000000000000000, 0.9510565162951535312, 1.000000000000000000, 0.9510565162951535312, 1.000000000000000000, 0.9510565162951535312, 1.000000000000000000, 0.9510565162951535312, 1.000000000000000000, 0.9510565162951535312, 1.000000000000000000, 0.9510565162951535312, 1.000000000000000000, 0.9510565162951535312, 1.000000000000000000, 0.9510565162951535312, 1.000000000000000000, 0.9510565162951535312, 1.000000000000000000, 0.9510565162951535312, 1.000000000000000000, 0.9510565162951535312, 1.000000000000000000, 0.9510565162951535312, 1.000000000000000000, 0.9510565162951535312, 1.000000000000000000, 0.9510565162951535312, 1.000000000000000000, 0.9510565162951535312, 1.000000000000000000, 0.9510565162951535312, 1.000000000000000000, 0.9510565162951535312, 1.000000000000000000, 0.9510565162951535312, 1.000000000000000000, 0.9510565162951535312, 1.000000000000000000, 0.9510565162951535312, 1.000000000000000000, 0.9510565162951535312, 1.000000000000000000, 0.9510565162951535312, 1.000000000000000000, 0.9510565162951535312, 1.000000000000000000, 0.9510565162951535312, 1.000000000000000000, 0.9510565162951535312, 1.000000000000000000, 0.9510565162951535312, 1.000000000000000000, 0.9510565162951535312, 1.000000000000000000, 0.9510565162951535312, 1.000000000000000000, 0.9510565162951535312, 1.000000000000000000, 0.9510565162951535312, 1.000000000000000000, 0.9510565162951535312, 1.000000000000000000, 0.9510565162951535312, 1.000000000000000000, 0.9510565162951535312, 1.000000000000000000, 0.9510565162951535312, 1.000000000000000000, 0.9510565162951535312, 1.000000000000000000, 0.9510565162951535312, 1.000000000000000000, 0.9510565162951535312, 1.000000000000000000, 0.9510565162951535312, 1.000000000000000000, 0.9510565162951535312, 1.000000000000000000, 0.9510565162951535312, 1.000000000000000000, 0.9510565162951535312, 1.000000000000000000, 0.9510565162951535312, 1.000000000000000000, 0.9510565162951535312, 1.000000000000000000, 0.9510565162951535312, 1.000000000000000000, 0.9510565162951535312, 1.000000000000000000, 0.9510565162951535312, 1.000000000000000000, 0.9510565162951535312, 1.000000000000000000, 0.9510565162951535312, 1.000000000000000000, 0.9510565162951535312, 1.000000000000000000, 0.9510565162951535312, 1.000000000000000000, 0.9510565162951535312, 1.000000000000000000, 0.9510565162951535312, 1.000000000000000000, 0.9510565162951535312, 1.000000000000000000, 0.9510565162951535312, 1.000000000000000000, 0.9510565162951535312, 1.000000000000000000, 0.9510565162951535312, 1.000000000000000000, 0.9510565162951535312, 1.000000000000000000, 0.9510565162951535312, 1.000000000000000000, 0.9510565162951535312, 1.000000000000000000, 0.9510565162951535312, 1.000000000000000000, 0.9510565162951535312, 1.000000000000000000, 0.9510565162951535312, 1.000000000000000000, 0.9510565162951535312, 1.000000000000000000, 0.9510565162951535312, 1.000000000000000000, 0.9510565162951535312, 1.000000000000000000, 0.9510565162951535312, 1.000000000000000000, 0.9510565162951535312, 1.000000000000000000, 0.9510565162951535312, 1.000000000000000000, 0.9510565162951535312, 1.000000000000000000, 0.9510565162951535312, 1.000000000000000000, 0.9510565162951535312, 1.000000000000000000, 0.9510565162951535312, 1.000000000000000000, 0.9510565162951535312, 1.000000000000000000, 0.9510565162951535312, 1.000000000000000000, 0.9510565162951535312, 1.000000000000000000, 0.9510565162951535312, 1.000000000000000000, 0.9510565162951535312, 1.000000000000000000, 0.9510565162951535312, 1.000000000000000000, 0.9510565162951535312, 1.000000000000000000, 0.9510565162951535312, 1.000000000000000000, 0.9510565162951535312, 1.000000000000000000, 0.9510565162951535312, 1.000000000000000000, 0.9510565162951535312, 1.000000000000000000, 0.9510565162951535312, 1.000000000000000000, 0.9510565162951535312, 1.000000000000000000, 0.9510565162951535312, 1.000000000000000000, 0.9510565162951535312, 1.000000000000000000, 0.9510565162951535312, 1.000000000000000000, 0.9510565162951535312, 1.000000000000000000, 0.9510565162951535312, 1.000000000000000000 ) ) 
 REPRESENTATION_ITEM ( '' )  );
#4323 = ORIENTED_EDGE ( 'NONE', *, *, #7727, .F. ) ;
#4324 = CARTESIAN_POINT ( 'NONE',  ( -4.243569643749998122, -21.91483169757570693, -11.28763325120213068 ) ) ;
#4325 = CARTESIAN_POINT ( 'NONE',  ( 2.733110507866247652, 33.87180007765647360, -3.862833514489153686 ) ) ;
#4326 = AXIS2_PLACEMENT_3D ( 'NONE', #14237, #8209, #9605 ) ;
#4327 = ORIENTED_EDGE ( 'NONE', *, *, #15402, .T. ) ;
#4328 = DIRECTION ( 'NONE',  ( 0.000000000000000000, 0.000000000000000000, 1.000000000000000000 ) ) ;
#4329 = DIRECTION ( 'NONE',  ( 1.000000000000000000, 0.000000000000000000, -0.000000000000000000 ) ) ;
#4330 = CARTESIAN_POINT ( 'NONE',  ( 4.299564228933482956E-15, -18.70396963712639504, -9.404344070490550322 ) ) ;
#4331 = CARTESIAN_POINT ( 'NONE',  ( -1.734723475976807094E-15, 40.79999999999999716, -2.500000000000000000 ) ) ;
#4332 = LINE ( 'NONE', #12338, #4350 ) ;
#4333 = CARTESIAN_POINT ( 'NONE',  ( 4.730628863548789710E-15, -17.11170270152969053, -8.699544261015072166 ) ) ;
#4334 = VERTEX_POINT ( 'NONE', #10293 ) ;
#4335 = CARTESIAN_POINT ( 'NONE',  ( 1.999999999999994449, -25.95818690119497418, -6.751175953542158936 ) ) ;
#4336 = ADVANCED_FACE ( 'NONE', ( #14386 ), #1690, .T. ) ;
#4337 = ORIENTED_EDGE ( 'NONE', *, *, #16762, .F. ) ;
#4338 = CIRCLE ( 'NONE', #14117, 0.9999999999999991118 ) ;
#4339 = ORIENTED_EDGE ( 'NONE', *, *, #2858, .F. ) ;
#4340 = CARTESIAN_POINT ( 'NONE',  ( -3.999999999999997335, -23.91744991381563779, -13.90249626042782971 ) ) ;
#4341 = FILL_AREA_STYLE ('',( #1309 ) ) ;
#4342 = CARTESIAN_POINT ( 'NONE',  ( -3.607379964056363075, 19.75319992234354416, -2.690724712371229899 ) ) ;
#4343 = CARTESIAN_POINT ( 'NONE',  ( 1.135272562821020070, 30.25319992234354416, -3.311245368580577164 ) ) ;
#4344 = CARTESIAN_POINT ( 'NONE',  ( 1.593127413382998903, 37.12180007765648071, 2.091722143975139669 ) ) ;
#4345 = VERTEX_POINT ( 'NONE', #8378 ) ;
#4346 = CARTESIAN_POINT ( 'NONE',  ( 0.05938372350919016857, 30.12819992234354061, -4.731580009072201776 ) ) ;
#4347 = CARTESIAN_POINT ( 'NONE',  ( 3.999999999999996447, -24.99080247827684431, -7.382766771737521161 ) ) ;
#4348 = ORIENTED_EDGE ( 'NONE', *, *, #13687, .F. ) ;
#4349 = DIRECTION ( 'NONE',  ( -0.000000000000000000, -0.5735764363510414965, -0.8191520442889950182 ) ) ;
#4350 = VECTOR ( 'NONE', #9979, 1000.000000000000000 ) ;
#4351 = CARTESIAN_POINT ( 'NONE',  ( 2.211161402132902243, 29.62180007765648071, 2.942372952327172442 ) ) ;
#4352 = CARTESIAN_POINT ( 'NONE',  ( -6.737340654859749201, -10.37508571686348269, 2.119921479756860183 ) ) ;
#4353 = CARTESIAN_POINT ( 'NONE',  ( 4.243569643750000786, -23.48083868096554028, -9.252632891433169249 ) ) ;
#4354 = EDGE_CURVE ( 'NONE', #5641, #11442, #7518, .T. ) ;
#4355 = CARTESIAN_POINT ( 'NONE',  ( 4.499999999999999112, 34.24680007765646650, -0.05647727720537982360 ) ) ;
#4356 = CARTESIAN_POINT ( 'NONE',  ( -1.734723475976807094E-15, 36.39999999999999147, -2.500000000000000000 ) ) ;
#4357 = ORIENTED_EDGE ( 'NONE', *, *, #1795, .T. ) ;
#4358 = EDGE_LOOP ( 'NONE', ( #826, #781, #10153, #5732 ) ) ;
#4359 = CARTESIAN_POINT ( 'NONE',  ( -3.518350579753630747, 25.62180007765648071, -1.080741659609802729 ) ) ;
#4360 = CARTESIAN_POINT ( 'NONE',  ( 6.428571428571432378, -14.26578344203647752, -2.827263138854379410 ) ) ;
#4361 = CARTESIAN_POINT ( 'NONE',  ( -2.000000000000005773, -29.67926403272728919, -12.06542484187378506 ) ) ;
#4362 = ORIENTED_EDGE ( 'NONE', *, *, #18253, .T. ) ;
#4363 =( GEOMETRIC_REPRESENTATION_CONTEXT ( 3 ) GLOBAL_UNCERTAINTY_ASSIGNED_CONTEXT ( ( #2502 ) ) GLOBAL_UNIT_ASSIGNED_CONTEXT ( ( #4384, #2914, #124 ) ) REPRESENTATION_CONTEXT ( 'NONE', 'WORKASPACE' ) );
#4364 = CARTESIAN_POINT ( 'NONE',  ( -3.518350579753605434, 16.87819992234353705, 1.080741659609877781 ) ) ;
#4365 = AXIS2_PLACEMENT_3D ( 'NONE', #10794, #1071, #8008 ) ;
#4366 = CARTESIAN_POINT ( 'NONE',  ( -4.243569643750005227, -24.30478114982620497, -6.157854574365327238 ) ) ;
#4367 = CARTESIAN_POINT ( 'NONE',  ( -3.500000000000000444, 40.49680007765648071, 0.05647727720536892260 ) ) ;
#4368 = CARTESIAN_POINT ( 'NONE',  ( 1.135272562821020070, 37.75319992234354061, -3.311245368580577164 ) ) ;
#4369 = CARTESIAN_POINT ( 'NONE',  ( 0.000000000000000000, 23.19999999999999574, 2.500000000000000000 ) ) ;
#4370 = LINE ( 'NONE', #116, #11715 ) ;
#4371 = CARTESIAN_POINT ( 'NONE',  ( 4.243569643749996345, -25.28344594435018067, -7.555532749933418835 ) ) ;
#4372 = VECTOR ( 'NONE', #6715, 1000.000000000000000 ) ;
#4373 = CIRCLE ( 'NONE', #18342, 0.9999999999999991118 ) ;
#4374 = AXIS2_PLACEMENT_3D ( 'NONE', #12071, #3918, #3824 ) ;
#4375 = EDGE_CURVE ( 'NONE', #12399, #16719, #13805, .T. ) ;
#4376 = AXIS2_PLACEMENT_3D ( 'NONE', #11978, #10496, #3555 ) ;
#4377 = CARTESIAN_POINT ( 'NONE',  ( 0.9156706748228305992, -9.999999999999090505, -4.445527249942534453 ) ) ;
#4378 = EDGE_CURVE ( 'NONE', #11183, #9839, #10448, .T. ) ;
#4379 = DIRECTION ( 'NONE',  ( 0.000000000000000000, 0.000000000000000000, 1.000000000000000000 ) ) ;
#4380 = DIRECTION ( 'NONE',  ( -0.000000000000000000, -1.000000000000000000, -0.000000000000000000 ) ) ;
#4381 = CARTESIAN_POINT ( 'NONE',  ( -2.121784821874996396, -18.06140184503912494, -7.920110144002082464 ) ) ;
#4382 = EDGE_CURVE ( 'NONE', #10740, #16544, #11408, .T. ) ;
#4383 = DIRECTION ( 'NONE',  ( 0.000000000000000000, 0.000000000000000000, -1.000000000000000000 ) ) ;
#4384 =( LENGTH_UNIT ( ) NAMED_UNIT ( * ) SI_UNIT ( .MILLI., .METRE. ) );
#4385 = EDGE_LOOP ( 'NONE', ( #2545, #13867, #3250, #11309 ) ) ;
#4386 = CARTESIAN_POINT ( 'NONE',  ( 0.05938372350921204690, 22.62819992234354771, -2.628655560595669183 ) ) ;
#4387 = EDGE_CURVE ( 'NONE', #12622, #11211, #16679, .T. ) ;
#4388 = DIRECTION ( 'NONE',  ( 0.000000000000000000, 0.000000000000000000, 1.000000000000000000 ) ) ;
#4389 = CARTESIAN_POINT ( 'NONE',  ( 3.481649420246369697, 19.12180007765648071, -1.193696214020541824 ) ) ;
#4390 = ADVANCED_FACE ( 'NONE', ( #17750 ), #12221, .T. ) ;
#4391 = TOROIDAL_SURFACE ( 'NONE', #12673, 2.200000000000000178, 0.2000000000000000111 ) ;
#4392 = LINE ( 'NONE', #14322, #9869 ) ;
#4393 = CIRCLE ( 'NONE', #5287, 3.799999999999999378 ) ;
#4394 = CIRCLE ( 'NONE', #13875, 0.9999999999999991118 ) ;
#4395 = CARTESIAN_POINT ( 'NONE',  ( 8.000000000000000000, 16.59999999999999787, -2.500000000000000888 ) ) ;
#4396 = EDGE_LOOP ( 'NONE', ( #6000, #5261, #9338, #7412 ) ) ;
#4397 = CARTESIAN_POINT ( 'NONE',  ( -2.121784821874996396, -17.06122793415199723, -6.491713766773147931 ) ) ;
#4398 = CARTESIAN_POINT ( 'NONE',  ( -1.027846397803541700, 34.99680007765648071, 3.346150245485522312 ) ) ;
#4399 = CARTESIAN_POINT ( 'NONE',  ( -2.121784821874996396, -23.77207223945918457, -16.07579268495438996 ) ) ;
#4400 = DIRECTION ( 'NONE',  ( 3.469446951953612217E-16, -0.000000000000000000, 1.000000000000000000 ) ) ;
#4401 = CARTESIAN_POINT ( 'NONE',  ( -4.243569643750000786, -25.15854975729233090, -11.64865262097848309 ) ) ;
#4402 = FACE_OUTER_BOUND ( 'NONE', #14788, .T. ) ;
#4403 = AXIS2_PLACEMENT_3D ( 'NONE', #2860, #5729, #3974 ) ;
#4404 = DIRECTION ( 'NONE',  ( -1.000000000000000000, -0.000000000000000000, -0.000000000000000000 ) ) ;
#4405 = CARTESIAN_POINT ( 'NONE',  ( 8.500000000000019540, 0.000000000000000000, 20.49999999999998934 ) ) ;
#4406 = CARTESIAN_POINT ( 'NONE',  ( 4.243569643749996345, -27.05794804431121037, -10.08978438695249835 ) ) ;
#4407 = FACE_OUTER_BOUND ( 'NONE', #9797, .T. ) ;
#4408 = CARTESIAN_POINT ( 'NONE',  ( 4.000000000000000888, -20.81908553137646578, -5.451255436407934418 ) ) ;
#4409 = CARTESIAN_POINT ( 'NONE',  ( 2.481649420246374138, 19.12180007765648071, -0.8687765177876252132 ) ) ;
#4410 = ORIENTED_EDGE ( 'NONE', *, *, #103, .F. ) ;
#4411 = CARTESIAN_POINT ( 'NONE',  ( -2.211161402132901799, 23.37180007765647716, -2.942372952327172886 ) ) ;
#4412 = CARTESIAN_POINT ( 'NONE',  ( -9.000000000000001776, 38.59999999999999432, 2.499999999999995559 ) ) ;
#4413 = DIRECTION ( 'NONE',  ( 1.000000000000000000, 0.000000000000000000, 0.000000000000000000 ) ) ;
#4414 = CARTESIAN_POINT ( 'NONE',  ( -10.00000000000000000, 43.00000000000000000, 2.499999999999996003 ) ) ;
#4415 = CARTESIAN_POINT ( 'NONE',  ( 1.593127413382953383, 35.37819992234354061, -2.091722143975172532 ) ) ;
#4416 = VERTEX_POINT ( 'NONE', #17565 ) ;
#4417 = CARTESIAN_POINT ( 'NONE',  ( 4.243569643750003451, -22.77519635210228088, -12.51636131763561721 ) ) ;
#4418 = VECTOR ( 'NONE', #12468, 1000.000000000000000 ) ;
#4419 = CARTESIAN_POINT ( 'NONE',  ( -4.481649420246366589, 30.37180007765647716, 1.518615910253458878 ) ) ;
#4420 = ORIENTED_EDGE ( 'NONE', *, *, #10628, .T. ) ;
#4421 = FACE_OUTER_BOUND ( 'NONE', #8555, .T. ) ;
#4422 = CARTESIAN_POINT ( 'NONE',  ( 1.071796769724495224, -19.48982452691913636, -10.52666116493661086 ) ) ;
#4423 = EDGE_CURVE ( 'NONE', #13234, #17672, #12513, .T. ) ;
#4424 = CARTESIAN_POINT ( 'NONE',  ( 4.000000000000003553, -20.13184543389877490, -8.496092768120460548 ) ) ;
#4425 = CARTESIAN_POINT ( 'NONE',  ( 2.199999999999999734, 0.000000000000000000, 0.000000000000000000 ) ) ;
#4426 = CARTESIAN_POINT ( 'NONE',  ( 10.00000000000000000, 23.19999999999999574, -2.500000000000003109 ) ) ;
#4427 = CARTESIAN_POINT ( 'NONE',  ( -5.330712181944245322E-15, -24.75231408233150887, -2.525507728232826210 ) ) ;
#4428 = ORIENTED_EDGE ( 'NONE', *, *, #16591, .T. ) ;
#4429 = VECTOR ( 'NONE', #12360, 1000.000000000000000 ) ;
#4430 = CYLINDRICAL_SURFACE ( 'NONE', #15624, 4.000000000000000000 ) ;
#4431 = CIRCLE ( 'NONE', #7691, 6.499999999999999112 ) ;
#4432 = ORIENTED_EDGE ( 'NONE', *, *, #10855, .F. ) ;
#4433 = VERTEX_POINT ( 'NONE', #1978 ) ;
#4434 =( BOUNDED_CURVE ( )  B_SPLINE_CURVE ( 2, ( #12856, #163, #5814, #10162, #9891, #4424, #7108, #3132, #4330 ),
 .UNSPECIFIED., .F., .T. ) 
 B_SPLINE_CURVE_WITH_KNOTS ( ( 3, 2, 2, 2, 3 ),
 ( 0.6810344827586206629, 0.6839080459770114917, 0.6896551724137931494, 0.6954022988505746961, 0.6982758620689655249 ),
 .UNSPECIFIED. ) 
 CURVE ( )  GEOMETRIC_REPRESENTATION_ITEM ( )  RATIONAL_B_SPLINE_CURVE ( ( 0.9330127018922194093, 0.9330127018922194093, 1.000000000000000000, 0.8660254037844387076, 1.000000000000000000, 0.8660254037844387076, 1.000000000000000000, 0.9330127018922194093, 0.9330127018922194093 ) ) 
 REPRESENTATION_ITEM ( '' )  );
#4435 = DIRECTION ( 'NONE',  ( 0.000000000000000000, 1.224646799147353207E-16, 1.000000000000000000 ) ) ;
#4436 = PRESENTATION_STYLE_ASSIGNMENT (( #16892 ) ) ;
#4437 = CARTESIAN_POINT ( 'NONE',  ( 2.829195390882724759, 17.87819992234354416, -3.793023760679264278 ) ) ;
#4438 = CARTESIAN_POINT ( 'NONE',  ( 2.211161402132839182, 25.37819992234354416, -2.942372952327217739 ) ) ;
#4439 = CARTESIAN_POINT ( 'NONE',  ( -2.518350579753628526, 38.12180007765647360, -0.7558219633769075463 ) ) ;
#4440 = ORIENTED_EDGE ( 'NONE', *, *, #14899, .T. ) ;
#4441 = CARTESIAN_POINT ( 'NONE',  ( -4.481649420246396787, 32.12819992234354771, -1.518615910253363399 ) ) ;
#4442 = CARTESIAN_POINT ( 'NONE',  ( 1.999999999999994449, -25.70007750483700448, -6.382557533612111200 ) ) ;
#4443 = ORIENTED_EDGE ( 'NONE', *, *, #3201, .F. ) ;
#4444 = EDGE_CURVE ( 'NONE', #16218, #16968, #9312, .T. ) ;
#4445 = CIRCLE ( 'NONE', #3868, 4.400000000000001243 ) ;
#4446 = DIRECTION ( 'NONE',  ( 0.000000000000000000, 0.000000000000000000, 1.000000000000000000 ) ) ;
#4447 = EDGE_CURVE ( 'NONE', #12413, #3919, #6601, .T. ) ;
#4448 = CARTESIAN_POINT ( 'NONE',  ( -2.115076519116362519, 27.62180007765648071, 3.012182706137107147 ) ) ;
#4449 = CARTESIAN_POINT ( 'NONE',  ( -7.191589934391295458, -10.00000000000000178, 14.52136967842656645 ) ) ;
#4450 = EDGE_CURVE ( 'NONE', #7294, #985, #16986, .T. ) ;
#4451 = CARTESIAN_POINT ( 'NONE',  ( 2.121784821875004390, -18.62063887048139321, -8.718783387183849598 ) ) ;
#4452 = CARTESIAN_POINT ( 'NONE',  ( -2.733110507866247652, 35.12180007765647360, 3.862833514489154574 ) ) ;
#4453 = EDGE_CURVE ( 'NONE', #3783, #634, #15210, .T. ) ;
#4454 = CARTESIAN_POINT ( 'NONE',  ( 4.898587196589415787E-16, 5.000000000000000000, -4.000000000000001776 ) ) ;
#4455 = ORIENTED_EDGE ( 'NONE', *, *, #12935, .T. ) ;
#4456 = EDGE_LOOP ( 'NONE', ( #10504, #7192, #11581, #5924 ) ) ;
#4457 = CARTESIAN_POINT ( 'NONE',  ( 3.481649420246369697, 21.62180007765647360, -1.193696214020541824 ) ) ;
#4458 = CARTESIAN_POINT ( 'NONE',  ( -4.000000000000003553, 6.938893903907228378E-15, 24.28148006742132026 ) ) ;
#4459 = SURFACE_SIDE_STYLE ('',( #7318 ) ) ;
#4460 = CARTESIAN_POINT ( 'NONE',  ( -4.000000000000004441, -23.33460051901814580, -5.017465244859820039 ) ) ;
#4461 = ORIENTED_EDGE ( 'NONE', *, *, #1895, .T. ) ;
#4462 = CARTESIAN_POINT ( 'NONE',  ( 1.027846397803612311, 16.25319992234354416, 3.346150245485499219 ) ) ;
#4463 = CARTESIAN_POINT ( 'NONE',  ( -4.000000000000004441, -28.23867904981954524, -12.02121522353072969 ) ) ;
#4464 = CARTESIAN_POINT ( 'NONE',  ( -4.243569643749997233, -20.85013043759908413, -9.767082268990684213 ) ) ;
#4465 = CARTESIAN_POINT ( 'NONE',  ( -1.135272562821090014, 35.99680007765648071, -3.311245368580554072 ) ) ;
#4466 = CARTESIAN_POINT ( 'NONE',  ( 1.027846397803612311, 31.25319992234354416, 3.346150245485499219 ) ) ;
#4467 = CARTESIAN_POINT ( 'NONE',  ( -4.000000000000004441, -23.07649112266017966, -4.648846824929771415 ) ) ;
#4468 = CARTESIAN_POINT ( 'NONE',  ( 4.000000000000003553, -23.03557614363086259, -12.64304999334026114 ) ) ;
#4469 = CARTESIAN_POINT ( 'NONE',  ( 4.243569643749996345, -24.76722715163424127, -6.818295910073324251 ) ) ;
#4470 = DIRECTION ( 'NONE',  ( 3.469446951953612217E-16, -0.000000000000000000, 1.000000000000000000 ) ) ;
#4471 = CIRCLE ( 'NONE', #1531, 0.9999999999999991118 ) ;
#4472 = CARTESIAN_POINT ( 'NONE',  ( -3.049298716197739623, -9.999999999999399591, -3.862741893372402036 ) ) ;
#4473 = DIRECTION ( 'NONE',  ( 6.162975822039154730E-33, -0.5735764363510414965, -0.8191520442889950182 ) ) ;
#4474 = CARTESIAN_POINT ( 'NONE',  ( -1.999999999999996225, -21.96064613819196154, -13.12104980222467532 ) ) ;
#4475 = CARTESIAN_POINT ( 'NONE',  ( -4.243569643750005227, -23.01423416803636002, -4.314762474715088558 ) ) ;
#4476 = CARTESIAN_POINT ( 'NONE',  ( -1.252219993090138761, 15.00000000000000355, -3.080002712724053904 ) ) ;
#4477 = SURFACE_STYLE_FILL_AREA ( #7622 ) ;
#4478 = VERTEX_POINT ( 'NONE', #13265 ) ;
#4479 = TOROIDAL_SURFACE ( 'NONE', #17239, 2.200000000000000178, 0.2000000000000000111 ) ;
#4480 = CARTESIAN_POINT ( 'NONE',  ( 0.05938372350921204690, 20.12819992234354771, -2.628655560595669183 ) ) ;
#4481 = DIRECTION ( 'NONE',  ( -0.000000000000000000, -1.000000000000000000, -0.000000000000000000 ) ) ;
#4482 = CARTESIAN_POINT ( 'NONE',  ( -14.99999999999999645, -10.00000000000000000, -30.00000000000000000 ) ) ;
#4483 = CARTESIAN_POINT ( 'NONE',  ( 3.607379964056306676, 18.99680007765647716, -2.690724712371305838 ) ) ;
#4484 = DIRECTION ( 'NONE',  ( -1.000000000000000000, -0.000000000000000000, -0.000000000000000000 ) ) ;
#4485 = AXIS2_PLACEMENT_3D ( 'NONE', #14640, #3588, #11928 ) ;
#4486 = DIRECTION ( 'NONE',  ( 0.000000000000000000, 0.000000000000000000, 1.000000000000000000 ) ) ;
#4487 = ORIENTED_EDGE ( 'NONE', *, *, #2542, .F. ) ;
#4488 = CARTESIAN_POINT ( 'NONE',  ( -4.243569643750000786, -20.28673490103567545, -4.690979944798832513 ) ) ;
#4489 = CARTESIAN_POINT ( 'NONE',  ( -2.211161402132902243, 33.37180007765648071, -2.942372952327172886 ) ) ;
#4490 = CARTESIAN_POINT ( 'NONE',  ( -5.330712181944245322E-15, -30.68883019856478711, -11.00373138662392236 ) ) ;
#4491 = TOROIDAL_SURFACE ( 'NONE', #6862, 9.000000000000001776, 0.9999999999999991118 ) ;
#4492 = DIRECTION ( 'NONE',  ( -0.000000000000000000, 1.000000000000000000, -0.000000000000000000 ) ) ;
#4493 = CARTESIAN_POINT ( 'NONE',  ( 2.121784821875004390, -22.23417041949295481, -13.87944126620451790 ) ) ;
#4494 = FACE_OUTER_BOUND ( 'NONE', #13704, .T. ) ;
#4495 = EDGE_CURVE ( 'NONE', #12374, #11611, #583, .T. ) ;
#4496 = AXIS2_PLACEMENT_3D ( 'NONE', #528, #5983, #247 ) ;
#4497 = FACE_OUTER_BOUND ( 'NONE', #7435, .T. ) ;
#4498 = DIRECTION ( 'NONE',  ( 1.000000000000000000, 0.000000000000000000, 0.000000000000000000 ) ) ;
#4499 = CARTESIAN_POINT ( 'NONE',  ( 4.730628863548789710E-15, -20.43486117963853843, -13.44550641761443366 ) ) ;
#4500 = LINE ( 'NONE', #10140, #18114 ) ;
#4501 = CARTESIAN_POINT ( 'NONE',  ( -3.999999999999997335, -19.07789873280867354, -6.990900887746200887 ) ) ;
#4502 = CARTESIAN_POINT ( 'NONE',  ( 2.055738996568313048, 19.49680007765648071, 1.423772053676023441 ) ) ;
#4503 = ORIENTED_EDGE ( 'NONE', *, *, #16967, .F. ) ;
#4504 = CARTESIAN_POINT ( 'NONE',  ( 2.211161402132902243, 22.12180007765648071, 2.942372952327172442 ) ) ;
#4505 = CARTESIAN_POINT ( 'NONE',  ( -2.000000000000005773, -25.03329489828385590, -5.430293283132924032 ) ) ;
#4506 = CARTESIAN_POINT ( 'NONE',  ( 0.000000000000000000, 0.000000000000000000, 0.000000000000000000 ) ) ;
#4507 = MECHANICAL_DESIGN_GEOMETRIC_PRESENTATION_REPRESENTATION (  '', ( #1851 ), #76 ) ;
#4508 = CARTESIAN_POINT ( 'NONE',  ( -9.000000000000003553, 31.99999999999999289, -2.500000000000001776 ) ) ;
#4509 = CARTESIAN_POINT ( 'NONE',  ( -0.05938372350921170689, 38.87819992234354771, 2.628655560595669183 ) ) ;
#4510 = ORIENTED_EDGE ( 'NONE', *, *, #13407, .T. ) ;
#4511 = CARTESIAN_POINT ( 'NONE',  ( -5.330712181944246111E-15, -27.84962683862713106, -6.948928767393399042 ) ) ;
#4512 = CARTESIAN_POINT ( 'NONE',  ( 4.481649420246366589, 34.12180007765647360, -1.518615910253458212 ) ) ;
#4513 = ORIENTED_EDGE ( 'NONE', *, *, #560, .F. ) ;
#4514 = DIRECTION ( 'NONE',  ( 1.000000000000000000, 0.000000000000000000, 0.000000000000000000 ) ) ;
#4515 = ADVANCED_FACE ( 'NONE', ( #17923, #10847, #13536, #4837, #6409, #7605 ), #3714, .T. ) ;
#4516 = DIRECTION ( 'NONE',  ( 1.000000000000000000, 0.000000000000000000, 0.000000000000000000 ) ) ;
#4517 = CARTESIAN_POINT ( 'NONE',  ( -2.121784821875005722, -28.67442979507872636, -10.26261452142547093 ) ) ;
#4518 = CARTESIAN_POINT ( 'NONE',  ( -4.000000000000007105, 6.938893903907228378E-15, -30.00000000000000000 ) ) ;
#4519 = AXIS2_PLACEMENT_3D ( 'NONE', #12054, #10760, #2163 ) ;
#4520 = LINE ( 'NONE', #11457, #17177 ) ;
#4521 = AXIS2_PLACEMENT_3D ( 'NONE', #7021, #6939, #11202 ) ;
#4522 = FACE_OUTER_BOUND ( 'NONE', #12486, .T. ) ;
#4523 = CARTESIAN_POINT ( 'NONE',  ( -4.243569643749997233, -19.33373773399602058, -7.601449051901653320 ) ) ;
#4524 = ORIENTED_EDGE ( 'NONE', *, *, #12834, .F. ) ;
#4525 = DIRECTION ( 'NONE',  ( -1.000000000000000000, -0.000000000000000000, -0.000000000000000000 ) ) ;
#4526 = CYLINDRICAL_SURFACE ( 'NONE', #8493, 0.9999999999999991118 ) ;
#4527 = ORIENTED_EDGE ( 'NONE', *, *, #16722, .F. ) ;
#4528 = ORIENTED_EDGE ( 'NONE', *, *, #17577, .F. ) ;
#4529 = CARTESIAN_POINT ( 'NONE',  ( 1.533898589781675205E-14, -27.51564321027552040, -8.041143755076902266 ) ) ;
#4530 = DIRECTION ( 'NONE',  ( 3.469446951953612217E-16, -0.000000000000000000, 1.000000000000000000 ) ) ;
#4531 = CARTESIAN_POINT ( 'NONE',  ( -1.336863392178569088, 15.00319992234354594, -4.297206761780648421 ) ) ;
#4532 = CARTESIAN_POINT ( 'NONE',  ( -2.864755990943222308, 24.25319992234354416, 2.011557305968548093 ) ) ;
#4533 = CARTESIAN_POINT ( 'NONE',  ( 2.500000000000001332, 36.74680007765648071, -0.05647727720535888202 ) ) ;
#4534 = AXIS2_PLACEMENT_3D ( 'NONE', #4508, #5985, #3034 ) ;
#4535 = VERTEX_POINT ( 'NONE', #6320 ) ;
#4536 = CARTESIAN_POINT ( 'NONE',  ( -4.518350579753602325, 34.37819992234354771, 1.405661355842794391 ) ) ;
#4537 = VECTOR ( 'NONE', #13445, 1000.000000000000000 ) ;
#4538 = CARTESIAN_POINT ( 'NONE',  ( 1.999999999999994449, -25.95818690119497418, -6.751175953542158936 ) ) ;
#4539 = ORIENTED_EDGE ( 'NONE', *, *, #16322, .T. ) ;
#4540 = CARTESIAN_POINT ( 'NONE',  ( 0.000000000000000000, 36.39999999999999147, 2.500000000000000000 ) ) ;
#4541 = CARTESIAN_POINT ( 'NONE',  ( 2.115076519116362963, 33.87180007765648071, -3.012182706137107147 ) ) ;
#4542 = CARTESIAN_POINT ( 'NONE',  ( -7.472465112787439523, -13.11650584547975917, 4.294891433530912295 ) ) ;
#4543 = CARTESIAN_POINT ( 'NONE',  ( -5.330712181944246111E-15, -25.23626920050269717, -3.216667265601667047 ) ) ;
#4544 = CARTESIAN_POINT ( 'NONE',  ( -4.499999999999999112, 27.99680007765647716, 0.05647727720537927543 ) ) ;
#4545 = VECTOR ( 'NONE', #10316, 1000.000000000000000 ) ;
#4546 = DIRECTION ( 'NONE',  ( -1.000000000000000000, 0.000000000000000000, -0.000000000000000000 ) ) ;
#4547 = VERTEX_POINT ( 'NONE', #7977 ) ;
#4548 = VERTEX_POINT ( 'NONE', #3629 ) ;
#4549 = CARTESIAN_POINT ( 'NONE',  ( -2.115076519116362519, 30.12180007765647360, 3.012182706137107147 ) ) ;
#4550 = CARTESIAN_POINT ( 'NONE',  ( -1.999999999999996225, -20.41198976004415044, -10.90933928264438890 ) ) ;
#4551 = EDGE_CURVE ( 'NONE', #11211, #16215, #4923, .T. ) ;
#4552 = DIRECTION ( 'NONE',  ( 0.000000000000000000, 0.000000000000000000, 1.000000000000000000 ) ) ;
#4553 = EDGE_LOOP ( 'NONE', ( #16641, #3896 ) ) ;
#4554 = CARTESIAN_POINT ( 'NONE',  ( 2.864755990943222308, 23.00319992234354416, -2.011557305968548093 ) ) ;
#4555 = EDGE_CURVE ( 'NONE', #4719, #9180, #7182, .T. ) ;
#4556 = DIRECTION ( 'NONE',  ( 0.000000000000000000, 0.5150380737757255245, 0.8571673013836856869 ) ) ;
#4557 = CARTESIAN_POINT ( 'NONE',  ( 2.121784821874994176, -24.21128814972218990, -3.888587676801722903 ) ) ;
#4558 = CARTESIAN_POINT ( 'NONE',  ( -2.798362969681365886, 40.24680007765648071, 2.102939460078824929 ) ) ;
#4559 = EDGE_CURVE ( 'NONE', #2896, #7772, #2254, .T. ) ;
#4560 = CARTESIAN_POINT ( 'NONE',  ( 3.481649420246394122, 30.87819992234353350, 1.193696214020467439 ) ) ;
#4561 = CARTESIAN_POINT ( 'NONE',  ( 1.999999999999994449, -29.82982784656450193, -12.28045225249287675 ) ) ;
#4562 = EDGE_CURVE ( 'NONE', #6875, #13000, #4322, .T. ) ;
#4563 = CARTESIAN_POINT ( 'NONE',  ( -4.243569643750000786, -22.86782886461536179, -8.377164144099308984 ) ) ;
#4564 = CARTESIAN_POINT ( 'NONE',  ( -1.848264997554276867, -10.00000000000000178, -4.668605916315860860 ) ) ;
#4565 = LINE ( 'NONE', #12731, #2403 ) ;
#4566 = DIRECTION ( 'NONE',  ( -0.000000000000000000, -0.5735764363510414965, -0.8191520442889950182 ) ) ;
#4567 = ORIENTED_EDGE ( 'NONE', *, *, #16232, .T. ) ;
#4568 = ORIENTED_EDGE ( 'NONE', *, *, #6775, .T. ) ;
#4569 = CARTESIAN_POINT ( 'NONE',  ( 2.121784821874994176, -23.95317875336422020, -3.519969256871676055 ) ) ;
#4570 = LINE ( 'NONE', #10027, #13898 ) ;
#4571 = SURFACE_STYLE_USAGE ( .BOTH. , #17305 ) ;
#4572 = EDGE_LOOP ( 'NONE', ( #3845, #5311, #5006, #5396 ) ) ;
#4573 = CARTESIAN_POINT ( 'NONE',  ( -2.518350579753611207, 16.87819992234354416, 0.7558219633769609480 ) ) ;
#4574 = CARTESIAN_POINT ( 'NONE',  ( -9.000000000000003553, 16.59999999999999787, -2.500000000000001776 ) ) ;
#4575 = CARTESIAN_POINT ( 'NONE',  ( -9.000000000000001776, 27.59999999999999432, 2.499999999999998224 ) ) ;
#4576 = DIRECTION ( 'NONE',  ( 1.000000000000000000, 0.000000000000000000, 0.000000000000000000 ) ) ;
#4577 = CARTESIAN_POINT ( 'NONE',  ( -3.706921591972381904E-14, -16.89720386262061425, -6.824015130980216171 ) ) ;
#4578 = VERTEX_POINT ( 'NONE', #16141 ) ;
#4579 = CARTESIAN_POINT ( 'NONE',  ( 3.518350579753631191, 36.87180007765645939, 1.080741659609802285 ) ) ;
#4580 = CARTESIAN_POINT ( 'NONE',  ( -4.243569643749997233, -24.49592566115538972, -14.97381745050260804 ) ) ;
#4581 = CARTESIAN_POINT ( 'NONE',  ( -1.071796769724486564, -28.30149810006826527, -9.163460849522957474 ) ) ;
#4582 = CARTESIAN_POINT ( 'NONE',  ( -4.243569643750000786, -25.93287794636623644, -12.75450788076862452 ) ) ;
#4583 = CARTESIAN_POINT ( 'NONE',  ( 0.000000000000000000, 5.977523610840987267, 32.81826849749789687 ) ) ;
#4584 = LINE ( 'NONE', #8941, #14518 ) ;
#4585 = DIRECTION ( 'NONE',  ( -0.000000000000000000, 1.000000000000000000, -0.000000000000000000 ) ) ;
#4586 = CARTESIAN_POINT ( 'NONE',  ( 4.243569643750000786, -25.28760445547132107, -11.83296183094350340 ) ) ;
#4587 = FACE_OUTER_BOUND ( 'NONE', #11356, .T. ) ;
#4588 = CARTESIAN_POINT ( 'NONE',  ( 4.000000000000003553, -18.13149761282945960, -5.639300014669354155 ) ) ;
#4589 = CARTESIAN_POINT ( 'NONE',  ( -2.500000000000001332, 22.99680007765648071, 0.05647727720535858364 ) ) ;
#4590 = VERTEX_POINT ( 'NONE', #2047 ) ;
#4591 = CARTESIAN_POINT ( 'NONE',  ( 3.481649420246370141, 21.62180007765647360, -1.193696214020541602 ) ) ;
#4592 = CARTESIAN_POINT ( 'NONE',  ( 3.999999999999996447, -25.82965801714518506, -8.580776637516944305 ) ) ;
#4593 = CARTESIAN_POINT ( 'NONE',  ( -3.999999999999997335, -23.72386786725210328, -13.62603244648705925 ) ) ;
#4594 = CARTESIAN_POINT ( 'NONE',  ( -8.500000000000010658, 15.00000000000000178, 20.49999999999998934 ) ) ;
#4595 = CARTESIAN_POINT ( 'NONE',  ( 3.500000000000000444, 18.25319992234354771, 0.05647727720529520379 ) ) ;
#4596 = ORIENTED_EDGE ( 'NONE', *, *, #7843, .T. ) ;
#4597 = CARTESIAN_POINT ( 'NONE',  ( 2.121784821874994176, -26.56653639148865409, -7.252230758663410271 ) ) ;
#4598 = CARTESIAN_POINT ( 'NONE',  ( 2.864755990943265829, 16.99680007765647716, 2.011557305968487697 ) ) ;
#4599 = ORIENTED_EDGE ( 'NONE', *, *, #12932, .F. ) ;
#4600 = DIRECTION ( 'NONE',  ( 1.000000000000000000, 0.000000000000000000, 0.000000000000000000 ) ) ;
#4601 = DIRECTION ( 'NONE',  ( -0.000000000000000000, -1.000000000000000000, -0.000000000000000000 ) ) ;
#4602 = CARTESIAN_POINT ( 'NONE',  ( -4.243569643750000786, -25.44892282819504459, -12.06334834339978634 ) ) ;
#4603 = FACE_OUTER_BOUND ( 'NONE', #671, .T. ) ;
#4604 = LINE ( 'NONE', #4798, #15994 ) ;
#4605 = CARTESIAN_POINT ( 'NONE',  ( -1.999999999999996225, -22.21875553454993124, -13.48966822215472305 ) ) ;
#4606 = CARTESIAN_POINT ( 'NONE',  ( 4.243569643750003451, -19.93599299216462484, -8.461558698405095669 ) ) ;
#4607 = VERTEX_POINT ( 'NONE', #13341 ) ;
#4608 = CARTESIAN_POINT ( 'NONE',  ( -1.071796769724486564, -28.04338870371029557, -8.794842429592909738 ) ) ;
#4609 = EDGE_CURVE ( 'NONE', #5374, #8582, #4899, .T. ) ;
#4610 = CARTESIAN_POINT ( 'NONE',  ( 3.999999999999996447, -22.92592730741309737, -4.433819412297139273 ) ) ;
#4611 = DIRECTION ( 'NONE',  ( -3.469446951953613696E-16, -0.000000000000000000, -1.000000000000000000 ) ) ;
#4612 = ORIENTED_EDGE ( 'NONE', *, *, #10558, .T. ) ;
#4613 = ORIENTED_EDGE ( 'NONE', *, *, #10319, .F. ) ;
#4614 = AXIS2_PLACEMENT_3D ( 'NONE', #4287, #5855, #8625 ) ;
#4615 = CARTESIAN_POINT ( 'NONE',  ( 0.000000000000000000, 33.00000000000000000, 0.000000000000000000 ) ) ;
#4616 = DIRECTION ( 'NONE',  ( -0.000000000000000000, -0.5735764363510414965, -0.8191520442889950182 ) ) ;
#4617 = CARTESIAN_POINT ( 'NONE',  ( 0.05938372350919016857, 30.12819992234354061, -4.731580009072201776 ) ) ;
#4618 = CARTESIAN_POINT ( 'NONE',  ( -3.500000000000000444, 29.50319992234354416, -0.05647727720529563400 ) ) ;
#4619 = EDGE_CURVE ( 'NONE', #12954, #16052, #8403, .T. ) ;
#4620 = AXIS2_PLACEMENT_3D ( 'NONE', #14260, #14447, #15744 ) ;
#4621 = CARTESIAN_POINT ( 'NONE',  ( 0.05938372350921204690, 22.62819992234354771, -2.628655560595669183 ) ) ;
#4622 = ORIENTED_EDGE ( 'NONE', *, *, #5925, .F. ) ;
#4623 = CARTESIAN_POINT ( 'NONE',  ( 3.607379964056363075, 31.00319992234354771, 2.690724712371229010 ) ) ;
#4624 = EDGE_CURVE ( 'NONE', #12442, #8755, #13702, .T. ) ;
#4625 = CARTESIAN_POINT ( 'NONE',  ( 2.000000000000004441, -18.64824221826470207, -8.390446746455726412 ) ) ;
#4626 = ORIENTED_EDGE ( 'NONE', *, *, #14416, .F. ) ;
#4627 = DIRECTION ( 'NONE',  ( 0.000000000000000000, 0.000000000000000000, -1.000000000000000000 ) ) ;
#4628 = CARTESIAN_POINT ( 'NONE',  ( -2.115076519116362519, 32.62180007765646650, 3.012182706137107147 ) ) ;
#4629 = CARTESIAN_POINT ( 'NONE',  ( -6.934387221018268654, -10.37764060375305064, 2.827117695748785131 ) ) ;
#4630 = CARTESIAN_POINT ( 'NONE',  ( -2.121784821875005722, -25.02863457152241722, -5.055879339913546211 ) ) ;
#4631 = AXIS2_PLACEMENT_3D ( 'NONE', #16370, #9150, #729 ) ;
#4632 = CARTESIAN_POINT ( 'NONE',  ( 1.444289557196047680, 27.24680007765647716, 4.262301884875704161 ) ) ;
#4633 = CARTESIAN_POINT ( 'NONE',  ( -8.500000000000005329, 14.99364916731036956, -18.35000000000000142 ) ) ;
#4634 = ORIENTED_EDGE ( 'NONE', *, *, #12813, .T. ) ;
#4635 = CARTESIAN_POINT ( 'NONE',  ( 0.05938372350927906274, 32.37180007765647360, 3.680117784833935701 ) ) ;
#4636 = CARTESIAN_POINT ( 'NONE',  ( -4.000000000000000888, -23.20659744698271965, -8.860975819754113303 ) ) ;
#4637 = CARTESIAN_POINT ( 'NONE',  ( 3.999999999999993339, 7.428752623566170548E-15, 30.00000000000000000 ) ) ;
#4638 = CARTESIAN_POINT ( 'NONE',  ( -4.000000000000004441, -28.43226109638308330, -12.29767903747149660 ) ) ;
#4639 = EDGE_LOOP ( 'NONE', ( #2393, #9544, #10796 ) ) ;
#4640 = CARTESIAN_POINT ( 'NONE',  ( 2.798362969681409851, 26.00319992234354771, 2.102939460078764977 ) ) ;
#4641 = DIRECTION ( 'NONE',  ( 0.000000000000000000, 0.000000000000000000, 1.000000000000000000 ) ) ;
#4642 = CARTESIAN_POINT ( 'NONE',  ( 4.243569643750000786, -20.89974471738585748, -5.566448692132691001 ) ) ;
#4643 = CARTESIAN_POINT ( 'NONE',  ( 1.135272562821090458, 39.74680007765648071, 3.311245368580554072 ) ) ;
#4644 = CARTESIAN_POINT ( 'NONE',  ( 2.115076519116426024, 31.12819992234354061, 3.012182706137062294 ) ) ;
#4645 = CARTESIAN_POINT ( 'NONE',  ( -4.243569643750000786, -26.73946980998488954, -13.90644044305002502 ) ) ;
#4646 = CIRCLE ( 'NONE', #11431, 0.9999999999999991118 ) ;
#4647 = CARTESIAN_POINT ( 'NONE',  ( 4.713407268011036227E-15, -22.84304572250594134, -16.39440596325204780 ) ) ;
#4648 = CARTESIAN_POINT ( 'NONE',  ( 2.121784821875004390, -19.42723073410004986, -9.870715949465248329 ) ) ;
#4649 = CARTESIAN_POINT ( 'NONE',  ( -2.343145750507623415, -3.999999999999993339, 11.59510085796834389 ) ) ;
#4650 = EDGE_CURVE ( 'NONE', #456, #2806, #6885, .T. ) ;
#4651 = EDGE_CURVE ( 'NONE', #6401, #11263, #2503, .T. ) ;
#4652 = DIRECTION ( 'NONE',  ( 0.000000000000000000, 0.000000000000000000, -1.000000000000000000 ) ) ;
#4653 = CARTESIAN_POINT ( 'NONE',  ( -10.00000000000000000, 16.59999999999999787, 2.499999999999996003 ) ) ;
#4654 = VECTOR ( 'NONE', #10888, 1000.000000000000000 ) ;
#4655 = FACE_OUTER_BOUND ( 'NONE', #15197, .T. ) ;
#4656 = ORIENTED_EDGE ( 'NONE', *, *, #1607, .T. ) ;
#4657 = ORIENTED_EDGE ( 'NONE', *, *, #9303, .F. ) ;
#4658 = CARTESIAN_POINT ( 'NONE',  ( -2.000000000000005773, -22.45220093470416955, -1.744109083832446894 ) ) ;
#4659 = DIRECTION ( 'NONE',  ( -0.000000000000000000, 1.000000000000000000, -0.000000000000000000 ) ) ;
#4660 = CARTESIAN_POINT ( 'NONE',  ( 4.299564228933482956E-15, -17.21984060877302269, -7.284788156899542066 ) ) ;
#4661 = VERTEX_POINT ( 'NONE', #10825 ) ;
#4662 = CARTESIAN_POINT ( 'NONE',  ( -2.055738996568281518, 29.25319992234355126, 1.423772053676066962 ) ) ;
#4663 = CARTESIAN_POINT ( 'NONE',  ( 4.243569643749996345, -27.31605744066918007, -10.45840280688254431 ) ) ;
#4664 = FACE_OUTER_BOUND ( 'NONE', #17182, .T. ) ;
#4665 = LINE ( 'NONE', #15899, #14331 ) ;
#4666 = CARTESIAN_POINT ( 'NONE',  ( -6.938893903907228378E-15, 6.938893903907228378E-15, 5.000000000000000888 ) ) ;
#4667 = ORIENTED_EDGE ( 'NONE', *, *, #15316, .F. ) ;
#4668 = CARTESIAN_POINT ( 'NONE',  ( 3.518350579753631191, 39.37180007765646650, 1.080741659609802285 ) ) ;
#4669 = CARTESIAN_POINT ( 'NONE',  ( -5.330712181944245322E-15, -30.17261140584885126, -10.26649454676382867 ) ) ;
#4670 = VECTOR ( 'NONE', #17689, 1000.000000000000000 ) ;
#4671 = EDGE_CURVE ( 'NONE', #8069, #10853, #15235, .T. ) ;
#4672 = EDGE_CURVE ( 'NONE', #9679, #6366, #6314, .T. ) ;
#4673 = CARTESIAN_POINT ( 'NONE',  ( -4.000000000000000888, -25.07789057128293919, -11.53345936525372650 ) ) ;
#4674 = ADVANCED_FACE ( 'NONE', ( #9432 ), #18177, .F. ) ;
#4675 = CARTESIAN_POINT ( 'NONE',  ( -4.243569643750004339, -25.85343752797401606, -8.369565093945613654 ) ) ;
#4676 = DIRECTION ( 'NONE',  ( 0.000000000000000000, 0.000000000000000000, 1.000000000000000000 ) ) ;
#4677 = CARTESIAN_POINT ( 'NONE',  ( 0.000000000000000000, 5.977523610840987267, 32.81826849749789687 ) ) ;
#4678 = DIRECTION ( 'NONE',  ( -0.000000000000000000, -0.5735764363510414965, -0.8191520442889950182 ) ) ;
#4679 = CARTESIAN_POINT ( 'NONE',  ( 2.121784821875004390, -20.16929524862920431, -10.93049390676413601 ) ) ;
#4680 = CARTESIAN_POINT ( 'NONE',  ( 4.000000000000003553, -19.93826338733523684, -8.219628954179688307 ) ) ;
#4681 = FACE_OUTER_BOUND ( 'NONE', #17306, .T. ) ;
#4682 =( GEOMETRIC_REPRESENTATION_CONTEXT ( 3 ) GLOBAL_UNCERTAINTY_ASSIGNED_CONTEXT ( ( #1038 ) ) GLOBAL_UNIT_ASSIGNED_CONTEXT ( ( #1383, #4058, #12678 ) ) REPRESENTATION_CONTEXT ( 'NONE', 'WORKASPACE' ) );
#4683 = CARTESIAN_POINT ( 'NONE',  ( -1.497042530366477164, 20.12180007765648071, 2.161531897785062384 ) ) ;
#4684 = VECTOR ( 'NONE', #282, 1000.000000000000000 ) ;
#4685 = AXIS2_PLACEMENT_3D ( 'NONE', #4934, #2178, #12340 ) ;
#4686 = ORIENTED_EDGE ( 'NONE', *, *, #1178, .F. ) ;
#4687 = CARTESIAN_POINT ( 'NONE',  ( -3.518350579753630303, 18.12180007765647716, -1.080741659609802952 ) ) ;
#4688 = CARTESIAN_POINT ( 'NONE',  ( 0.000000000000000000, 13.00000000000000178, -6.499999999999999112 ) ) ;
#4689 = CARTESIAN_POINT ( 'NONE',  ( -1.999999999999996225, -23.05761107341827199, -14.68767808793413998 ) ) ;
#4690 = PLANE ( 'NONE',  #7789 ) ;
#4691 = CARTESIAN_POINT ( 'NONE',  ( 2.864755990943222308, 20.50319992234354416, -2.011557305968548093 ) ) ;
#4692 = EDGE_LOOP ( 'NONE', ( #13063, #15901, #167, #9863 ) ) ;
#4693 = CARTESIAN_POINT ( 'NONE',  ( 2.121784821874994176, -26.30842699513068439, -6.883612338733362535 ) ) ;
#4694 = CARTESIAN_POINT ( 'NONE',  ( 2.115076519116362963, 18.87180007765648071, -3.012182706137107147 ) ) ;
#4695 = VERTEX_POINT ( 'NONE', #5265 ) ;
#4696 =( NAMED_UNIT ( * ) SI_UNIT ( $, .STERADIAN. ) SOLID_ANGLE_UNIT ( ) );
#4697 = CIRCLE ( 'NONE', #2643, 6.499999999999999112 ) ;
#4698 = FACE_OUTER_BOUND ( 'NONE', #1877, .T. ) ;
#4699 = CARTESIAN_POINT ( 'NONE',  ( 4.730628863548789710E-15, -21.24145304325719152, -14.59743897989583594 ) ) ;
#4700 = CARTESIAN_POINT ( 'NONE',  ( 3.999999999999996447, -28.60433402728840591, -12.54342465075819035 ) ) ;
#4701 = LINE ( 'NONE', #15745, #13005 ) ;
#4702 = CARTESIAN_POINT ( 'NONE',  ( 3.999999999999996447, -25.57154862078721891, -8.212158217586894793 ) ) ;
#4703 =( BOUNDED_CURVE ( )  B_SPLINE_CURVE ( 2, ( #4139, #5439, #15468, #8309, #6733, #16771, #11086, #6913, #17042 ),
 .UNSPECIFIED., .F., .T. ) 
 B_SPLINE_CURVE_WITH_KNOTS ( ( 3, 2, 2, 2, 3 ),
 ( 0.4913793103448276245, 0.4942528735632183978, 0.5000000000000000000, 0.5057471264367816577, 0.5086206896551724865 ),
 .UNSPECIFIED. ) 
 CURVE ( )  GEOMETRIC_REPRESENTATION_ITEM ( )  RATIONAL_B_SPLINE_CURVE ( ( 0.9330127018922194093, 0.9330127018922200755, 1.000000000000000000, 0.8660254037844387076, 1.000000000000000000, 0.8660254037844387076, 1.000000000000000000, 0.9330127018922180770, 0.9330127018922194093 ) ) 
 REPRESENTATION_ITEM ( '' )  );
#4704 = CARTESIAN_POINT ( 'NONE',  ( -4.243569643750005227, -23.04649784258110756, -4.360839777206344081 ) ) ;
#4705 = ORIENTED_EDGE ( 'NONE', *, *, #10684, .T. ) ;
#4706 = FACE_OUTER_BOUND ( 'NONE', #4997, .T. ) ;
#4707 = EDGE_CURVE ( 'NONE', #526, #13373, #13999, .T. ) ;
#4708 = CARTESIAN_POINT ( 'NONE',  ( -3.706921591972381904E-14, -18.96207903348436119, -9.772962490420598058 ) ) ;
#4709 = LINE ( 'NONE', #10072, #18017 ) ;
#4710 = VERTEX_POINT ( 'NONE', #2772 ) ;
#4711 = ORIENTED_EDGE ( 'NONE', *, *, #7028, .F. ) ;
#4712 = CARTESIAN_POINT ( 'NONE',  ( 4.000000000000003553, -22.26124795455695704, -11.53719473355011793 ) ) ;
#4713 = DIRECTION ( 'NONE',  ( 0.5735764363510414965, -0.6710100716628397688, 0.4698463103929523821 ) ) ;
#4714 = AXIS2_PLACEMENT_3D ( 'NONE', #13224, #11834, #4795 ) ;
#4715 = CARTESIAN_POINT ( 'NONE',  ( -2.829195390882724315, 24.12819992234354771, 3.793023760679264722 ) ) ;
#4716 = CARTESIAN_POINT ( 'NONE',  ( -0.05938372350920064630, 36.37819992234354771, 3.680117784833935701 ) ) ;
#4717 = VECTOR ( 'NONE', #13801, 1000.000000000000000 ) ;
#4718 = CARTESIAN_POINT ( 'NONE',  ( 1.593127413382953383, 22.87819992234354771, -2.091722143975172532 ) ) ;
#4719 = VERTEX_POINT ( 'NONE', #3875 ) ;
#4720 = CARTESIAN_POINT ( 'NONE',  ( 4.481649420246366589, 19.12180007765647360, -1.518615910253458212 ) ) ;
#4721 = CARTESIAN_POINT ( 'NONE',  ( -4.000000000000004441, -24.04440135829761616, -6.031165898660685087 ) ) ;
#4722 = EDGE_LOOP ( 'NONE', ( #4050, #7068, #2960, #12915 ) ) ;
#4723 = CARTESIAN_POINT ( 'NONE',  ( 0.000000000000000000, 31.99999999999999289, 2.500000000000000000 ) ) ;
#4724 = CARTESIAN_POINT ( 'NONE',  ( -2.115076519116362519, 30.12180007765647360, 3.012182706137107147 ) ) ;
#4725 = EDGE_CURVE ( 'NONE', #2518, #5641, #553, .T. ) ;
#4726 = LINE ( 'NONE', #6306, #16419 ) ;
#4727 = AXIS2_PLACEMENT_3D ( 'NONE', #14450, #5905, #11554 ) ;
#4728 = CARTESIAN_POINT ( 'NONE',  ( 4.730628863548789710E-15, -18.11187661241681823, -10.12794063824400581 ) ) ;
#4729 = CIRCLE ( 'NONE', #10647, 5.000000000000000000 ) ;
#4730 = CARTESIAN_POINT ( 'NONE',  ( -4.481649420246366589, 32.87180007765647360, 1.518615910253458878 ) ) ;
#4731 = EDGE_CURVE ( 'NONE', #12052, #1787, #8315, .T. ) ;
#4732 = DIRECTION ( 'NONE',  ( -0.000000000000000000, -1.000000000000000000, -0.000000000000000000 ) ) ;
#4733 = ORIENTED_EDGE ( 'NONE', *, *, #14526, .T. ) ;
#4734 = CARTESIAN_POINT ( 'NONE',  ( 1.027846397803542144, 33.74680007765648071, -3.346150245485522312 ) ) ;
#4735 = CARTESIAN_POINT ( 'NONE',  ( 1.522508701836648326, -10.00000000000000178, 22.87631747053914211 ) ) ;
#4736 = CARTESIAN_POINT ( 'NONE',  ( 1.533898589781675205E-14, -26.99942441755958811, -7.303906915216807683 ) ) ;
#4737 = CARTESIAN_POINT ( 'NONE',  ( 4.433153569487552126, -10.00000000000000000, 28.39434458091830393 ) ) ;
#4738 = CARTESIAN_POINT ( 'NONE',  ( 4.299564228933482956E-15, -23.34993877156982833, -16.03947562923141135 ) ) ;
#4739 = ORIENTED_EDGE ( 'NONE', *, *, #7940, .T. ) ;
#4740 = CARTESIAN_POINT ( 'NONE',  ( -2.115076519116425580, 24.87819992234354771, -3.012182706137062738 ) ) ;
#4741 = DIRECTION ( 'NONE',  ( -1.000000000000000000, 0.000000000000000000, 0.000000000000000000 ) ) ;
#4742 = CARTESIAN_POINT ( 'NONE',  ( -4.243569643749997233, -18.78525526673533719, -6.818134909550300549 ) ) ;
#4743 = CARTESIAN_POINT ( 'NONE',  ( 0.7188294034286049072, 18.74680007765648071, -2.395093729190366005 ) ) ;
#4744 = CIRCLE ( 'NONE', #10947, 2.499999999999999556 ) ;
#4745 = CARTESIAN_POINT ( 'NONE',  ( 4.481649420246397675, 18.37819992234354416, 1.518615910253363177 ) ) ;
#4746 = DIRECTION ( 'NONE',  ( 3.469446951953612217E-16, -0.000000000000000000, 1.000000000000000000 ) ) ;
#4747 = CARTESIAN_POINT ( 'NONE',  ( -4.000000000000004441, -27.91604230366714390, -11.56044219761140290 ) ) ;
#4748 = CARTESIAN_POINT ( 'NONE',  ( -4.243569643749997233, -19.59184713035399383, -7.970067471831701056 ) ) ;
#4749 = CARTESIAN_POINT ( 'NONE',  ( -1.734723475976807094E-15, 18.79999999999999361, -11.50000000000000178 ) ) ;
#4750 = EDGE_CURVE ( 'NONE', #9690, #10864, #2779, .T. ) ;
#4751 = CARTESIAN_POINT ( 'NONE',  ( -4.778136680858375840, -10.00000000000000178, -10.60429372729901054 ) ) ;
#4752 = CIRCLE ( 'NONE', #11856, 6.499999999999999112 ) ;
#4753 = DIRECTION ( 'NONE',  ( 0.000000000000000000, 0.000000000000000000, -1.000000000000000000 ) ) ;
#4754 = CARTESIAN_POINT ( 'NONE',  ( 2.599319604203554679, -24.48737926485759431, -15.99075565718284153 ) ) ;
#4755 = ORIENTED_EDGE ( 'NONE', *, *, #3440, .T. ) ;
#4756 = ORIENTED_EDGE ( 'NONE', *, *, #12726, .F. ) ;
#4757 = CARTESIAN_POINT ( 'NONE',  ( 2.121784821874994176, -22.66263177157437525, -1.676877157221437376 ) ) ;
#4758 = APPLICATION_CONTEXT ( 'automotive_design' ) ;
#4759 = ORIENTED_EDGE ( 'NONE', *, *, #2383, .F. ) ;
#4760 = CARTESIAN_POINT ( 'NONE',  ( 1.497042530366522461, 31.12819992234354416, 2.161531897785029965 ) ) ;
#4761 = CARTESIAN_POINT ( 'NONE',  ( -5.330712181944245322E-15, -29.36601954223019462, -9.114561984482429935 ) ) ;
#4762 = CARTESIAN_POINT ( 'NONE',  ( -1.135272562821090014, 23.49680007765647716, -3.311245368580554072 ) ) ;
#4763 = CARTESIAN_POINT ( 'NONE',  ( 4.000000000000000000, 1.759474945355387954, 3.047499999999997211 ) ) ;
#4764 = CARTESIAN_POINT ( 'NONE',  ( 3.412954772041557838, -15.19080604886703512, -9.070274817126225742 ) ) ;
#4765 = CIRCLE ( 'NONE', #11266, 0.9999999999999991118 ) ;
#4766 = CARTESIAN_POINT ( 'NONE',  ( 2.115076519116362963, 38.87180007765645939, -3.012182706137107147 ) ) ;
#4767 = CARTESIAN_POINT ( 'NONE',  ( -2.121784821875005722, -28.41632039872075666, -9.893996101495421414 ) ) ;
#4768 = CARTESIAN_POINT ( 'NONE',  ( -8.500000000000005329, 10.00000000000000000, -20.49999999999999645 ) ) ;
#4769 = CARTESIAN_POINT ( 'NONE',  ( 2.121784821875004390, -21.71795162677701896, -13.14220442634442243 ) ) ;
#4770 = DIRECTION ( 'NONE',  ( -0.000000000000000000, 1.000000000000000000, -0.000000000000000000 ) ) ;
#4771 = B_SPLINE_CURVE_WITH_KNOTS ( 'NONE', 3,
 ( #5752, #17364, #7129, #14190, #16995, #7, #10087, #4269, #13066, #9912, #97, #11389, #381, #17080 ),
 .UNSPECIFIED., .F., .F.,
 ( 4, 2, 2, 2, 2, 2, 4 ),
 ( 0.000000000000000000, 0.004742253375847067971, 0.007113380063770602391, 0.009484506751694135943, 0.01422676012754120478, 0.01659788681546473660, 0.01896901350338827189 ),
 .UNSPECIFIED. ) ;
#4772 = DIRECTION ( 'NONE',  ( 0.000000000000000000, 0.5150380737757255245, 0.8571673013836856869 ) ) ;
#4773 = DIRECTION ( 'NONE',  ( -0.000000000000000000, -1.000000000000000000, -0.000000000000000000 ) ) ;
#4774 = CARTESIAN_POINT ( 'NONE',  ( -4.243569643750000786, -22.83556519007061425, -8.331086841608051685 ) ) ;
#4775 = CARTESIAN_POINT ( 'NONE',  ( -8.000000000000001776, 34.19999999999999574, 2.499999999999998224 ) ) ;
#4776 = CARTESIAN_POINT ( 'NONE',  ( 4.000000000000000000, -1.759474945355381292, 3.047500000000002540 ) ) ;
#4777 = CARTESIAN_POINT ( 'NONE',  ( -2.055738996568313048, 28.24680007765648071, -1.423772053676023441 ) ) ;
#4778 = ORIENTED_EDGE ( 'NONE', *, *, #5020, .F. ) ;
#4779 = CARTESIAN_POINT ( 'NONE',  ( -3.518350579753630303, 30.62180007765647716, -1.080741659609802952 ) ) ;
#4780 = CARTESIAN_POINT ( 'NONE',  ( -10.00000000000000000, 27.59999999999999432, 2.499999999999996003 ) ) ;
#4781 = EDGE_CURVE ( 'NONE', #1579, #1028, #3655, .T. ) ;
#4782 =( NAMED_UNIT ( * ) PLANE_ANGLE_UNIT ( ) SI_UNIT ( $, .RADIAN. ) );
#4783 = CARTESIAN_POINT ( 'NONE',  ( -5.279047395330986450E-15, -29.05497384477128975, -9.160687100776456759 ) ) ;
#4784 = CARTESIAN_POINT ( 'NONE',  ( 20.00000000000000355, 0.000000000000000000, 0.000000000000000000 ) ) ;
#4785 = EDGE_CURVE ( 'NONE', #4548, #3027, #701, .T. ) ;
#4786 = CARTESIAN_POINT ( 'NONE',  ( 0.05938372350920109732, 17.62819992234354771, -3.680117784833935701 ) ) ;
#4787 = ORIENTED_EDGE ( 'NONE', *, *, #11122, .T. ) ;
#4788 = CARTESIAN_POINT ( 'NONE',  ( 2.121784821874994176, -26.05031759877271469, -6.514993918803313910 ) ) ;
#4789 = ADVANCED_FACE ( 'NONE', ( #12576 ), #6621, .F. ) ;
#4790 = CARTESIAN_POINT ( 'NONE',  ( 1.135272562821090458, 17.24680007765647716, 3.311245368580554072 ) ) ;
#4791 = ORIENTED_EDGE ( 'NONE', *, *, #950, .T. ) ;
#4792 = ADVANCED_FACE ( 'NONE', ( #12934 ), #1737, .F. ) ;
#4793 = CARTESIAN_POINT ( 'NONE',  ( 1.820000000000000062, 3.799999999999999378, 0.000000000000000000 ) ) ;
#4794 = VECTOR ( 'NONE', #13323, 1000.000000000000000 ) ;
#4795 = DIRECTION ( 'NONE',  ( 0.000000000000000000, 0.000000000000000000, 1.000000000000000000 ) ) ;
#4796 = CARTESIAN_POINT ( 'NONE',  ( -2.121784821875005722, -28.41632039872075666, -9.893996101495421414 ) ) ;
#4797 = AXIS2_PLACEMENT_3D ( 'NONE', #17933, #16813, #10950 ) ;
#4798 = CARTESIAN_POINT ( 'NONE',  ( -14.99999999999999645, 10.00000000000000000, 30.00000000000000000 ) ) ;
#4799 = CARTESIAN_POINT ( 'NONE',  ( 1.071796769724485454, -20.32868006578746645, -11.72467103071603134 ) ) ;
#4800 = CARTESIAN_POINT ( 'NONE',  ( 2.121784821875004390, -24.04093619399873560, -16.45977020571485028 ) ) ;
#4801 = ADVANCED_FACE ( 'NONE', ( #1551 ), #9965, .T. ) ;
#4802 = EDGE_LOOP ( 'NONE', ( #11395, #4440, #5564, #15802 ) ) ;
#4803 = CARTESIAN_POINT ( 'NONE',  ( -3.999999999999997335, -21.65899269638835634, -10.67708508704667558 ) ) ;
#4804 = AXIS2_PLACEMENT_3D ( 'NONE', #18011, #6670, #9811 ) ;
#4805 = CARTESIAN_POINT ( 'NONE',  ( 3.999999999999996447, -25.31343922442924921, -7.843539797656847057 ) ) ;
#4806 = AXIS2_PLACEMENT_3D ( 'NONE', #4097, #15514, #2726 ) ;
#4807 = DIRECTION ( 'NONE',  ( 0.000000000000000000, 0.000000000000000000, 1.000000000000000000 ) ) ;
#4808 = VERTEX_POINT ( 'NONE', #8482 ) ;
#4809 = VERTEX_POINT ( 'NONE', #15829 ) ;
#4810 = CARTESIAN_POINT ( 'NONE',  ( -13.00000000000000178, 15.00000000000000178, 16.00000000000000000 ) ) ;
#4811 = PRODUCT_RELATED_PRODUCT_CATEGORY ( 'part', '', ( #3977 ) ) ;
#4812 = CARTESIAN_POINT ( 'NONE',  ( 4.299564228933482956E-15, -16.44551241969911359, -6.178932897109397970 ) ) ;
#4813 = CARTESIAN_POINT ( 'NONE',  ( -1.661723472263481630E-14, -20.31715336506863778, -11.70820919606011579 ) ) ;
#4814 = CARTESIAN_POINT ( 'NONE',  ( -4.518350579753602325, 24.37819992234354416, 1.405661355842794391 ) ) ;
#4815 = CARTESIAN_POINT ( 'NONE',  ( 2.798362969681409851, 38.50319992234354061, 2.102939460078764977 ) ) ;
#4816 = CARTESIAN_POINT ( 'NONE',  ( -2.500000000000001332, 17.00319992234354416, -0.05647727720530596601 ) ) ;
#4817 = ORIENTED_EDGE ( 'NONE', *, *, #1277, .F. ) ;
#4818 = CARTESIAN_POINT ( 'NONE',  ( -2.829195390882805139, 20.87180007765647716, -3.793023760679206102 ) ) ;
#4819 = CARTESIAN_POINT ( 'NONE',  ( -2.000000000000005773, -25.48498634120535655, -6.075375517003743120 ) ) ;
#4820 = EDGE_LOOP ( 'NONE', ( #15015, #16241, #7135, #13282, #7186 ) ) ;
#4821 = AXIS2_PLACEMENT_3D ( 'NONE', #827, #10733, #7767 ) ;
#4822 = CARTESIAN_POINT ( 'NONE',  ( 10.00000000000000000, 40.79999999999999716, -2.500000000000003109 ) ) ;
#4823 = DIRECTION ( 'NONE',  ( -0.000000000000000000, 1.000000000000000000, -0.000000000000000000 ) ) ;
#4824 =( BOUNDED_CURVE ( )  B_SPLINE_CURVE ( 2, ( #1241, #2895, #9838, #14110, #17009, #8531, #4361, #5401, #12621 ),
 .UNSPECIFIED., .F., .T. ) 
 B_SPLINE_CURVE_WITH_KNOTS ( ( 3, 2, 2, 2, 3 ),
 ( 0.008620689655172418878, 0.01149425287356321823, 0.01724137931034482735, 0.02298850574712643646, 0.02586206896551724449 ),
 .UNSPECIFIED. ) 
 CURVE ( )  GEOMETRIC_REPRESENTATION_ITEM ( )  RATIONAL_B_SPLINE_CURVE ( ( 0.9330127018922192983, 0.9330127018922194093, 1.000000000000000000, 0.8660254037844387076, 1.000000000000000000, 0.8660254037844387076, 1.000000000000000000, 0.9330127018922191873, 0.9330127018922194093 ) ) 
 REPRESENTATION_ITEM ( '' )  );
#4825 = CARTESIAN_POINT ( 'NONE',  ( 9.000000000000005329, -13.00000000000000178, 15.14468620625654616 ) ) ;
#4826 = CARTESIAN_POINT ( 'NONE',  ( 4.243569643750000786, -21.67407290645975948, -6.672303951922835097 ) ) ;
#4827 = MECHANICAL_DESIGN_GEOMETRIC_PRESENTATION_REPRESENTATION (  '', ( #8072 ), #16407 ) ;
#4828 = CARTESIAN_POINT ( 'NONE',  ( 4.730628863548789710E-15, -20.20901545782531628, -13.12296530017564500 ) ) ;
#4829 = ORIENTED_EDGE ( 'NONE', *, *, #10457, .T. ) ;
#4830 = CARTESIAN_POINT ( 'NONE',  ( -1.071796769724477238, -23.07478282311446449, -1.698937844932721708 ) ) ;
#4831 = CARTESIAN_POINT ( 'NONE',  ( 8.500000000000001776, 15.00000000000000000, -20.49999999999999645 ) ) ;
#4832 = DIRECTION ( 'NONE',  ( 0.000000000000000000, 0.000000000000000000, -1.000000000000000000 ) ) ;
#4833 = SURFACE_STYLE_USAGE ( .BOTH. , #1687 ) ;
#4834 = EDGE_LOOP ( 'NONE', ( #14359, #2699, #623, #14473 ) ) ;
#4835 = AXIS2_PLACEMENT_3D ( 'NONE', #7415, #9087, #14767 ) ;
#4836 = CARTESIAN_POINT ( 'NONE',  ( 2.115076519116426024, 28.62819992234353705, 3.012182706137062294 ) ) ;
#4837 = FACE_OUTER_BOUND ( 'NONE', #16452, .T. ) ;
#4838 = CARTESIAN_POINT ( 'NONE',  ( 2.121784821875004390, -18.10442007776545736, -7.981546547323755014 ) ) ;
#4839 = CARTESIAN_POINT ( 'NONE',  ( 1.497042530366477164, 21.37180007765648071, -2.161531897785062384 ) ) ;
#4840 = CARTESIAN_POINT ( 'NONE',  ( 3.673772985318163098, 20.50319992234354771, -2.599342558261029001 ) ) ;
#4841 = CARTESIAN_POINT ( 'NONE',  ( 4.243569643750003451, -24.32385273025008843, -14.72807183721590718 ) ) ;
#4842 = CARTESIAN_POINT ( 'NONE',  ( 2.000000000000004441, -23.81043014542407121, -15.76281514505668113 ) ) ;
#4843 = CARTESIAN_POINT ( 'NONE',  ( 4.243569643750000786, -20.93200839193060148, -5.612525994623947412 ) ) ;
#4844 = CARTESIAN_POINT ( 'NONE',  ( 0.000000000000000000, 29.79999999999999716, 2.500000000000000000 ) ) ;
#4845 = AXIS2_PLACEMENT_3D ( 'NONE', #17879, #6540, #5148 ) ;
#4846 = CARTESIAN_POINT ( 'NONE',  ( -3.999999999999997335, -23.65934051745766808, -13.53387784049778197 ) ) ;
#4847 = CYLINDRICAL_SURFACE ( 'NONE', #12147, 4.000000000000000000 ) ;
#4848 = DIRECTION ( 'NONE',  ( 0.000000000000000000, 0.000000000000000000, -1.000000000000000000 ) ) ;
#4849 = ORIENTED_EDGE ( 'NONE', *, *, #17388, .T. ) ;
#4850 = ORIENTED_EDGE ( 'NONE', *, *, #3092, .F. ) ;
#4851 = CARTESIAN_POINT ( 'NONE',  ( -1.734723475976807094E-15, 25.39999999999999503, -11.50000000000000178 ) ) ;
#4852 = FILL_AREA_STYLE_COLOUR ( '', #6157 ) ;
#4853 = ORIENTED_EDGE ( 'NONE', *, *, #11225, .F. ) ;
#4854 = CARTESIAN_POINT ( 'NONE',  ( -1.989345975306457071, 27.25319992234354771, -1.515154207786300944 ) ) ;
#4855 = PRESENTATION_STYLE_ASSIGNMENT (( #17592 ) ) ;
#4856 = CARTESIAN_POINT ( 'NONE',  ( 2.121784821875004390, -22.75038921220889065, -14.61667810606461337 ) ) ;
#4857 = CARTESIAN_POINT ( 'NONE',  ( -1.135272562821090014, 25.99680007765648071, -3.311245368580554072 ) ) ;
#4858 = AXIS2_PLACEMENT_3D ( 'NONE', #6246, #17595, #10510 ) ;
#4859 = PRODUCT ( 'Return Spring', 'Return Spring', '', ( #16294 ) ) ;
#4860 = CARTESIAN_POINT ( 'NONE',  ( 0.000000000000000000, 9.254131787996968228, 30.52396275209373044 ) ) ;
#4861 = EDGE_CURVE ( 'NONE', #1681, #17541, #13416, .T. ) ;
#4862 = CARTESIAN_POINT ( 'NONE',  ( -0.2621597573796389802, -10.00000000000313527, -3.075850967169316164 ) ) ;
#4863 = CARTESIAN_POINT ( 'NONE',  ( -4.243569643749997233, -23.46348807572352158, -13.49934377078241710 ) ) ;
#4864 = CARTESIAN_POINT ( 'NONE',  ( -4.243569643749998122, -21.62445862667299323, -10.87293752878082742 ) ) ;
#4865 = FACE_OUTER_BOUND ( 'NONE', #2268, .T. ) ;
#4866 = CARTESIAN_POINT ( 'NONE',  ( -1.734723475976807094E-15, 25.39999999999999503, -2.500000000000000000 ) ) ;
#4867 = CARTESIAN_POINT ( 'NONE',  ( 4.005420803925811235, -27.01550616763517709, -14.30066121701663029 ) ) ;
#4868 = CARTESIAN_POINT ( 'NONE',  ( -2.121784821875005722, -26.83540034602819802, -7.636208279423879475 ) ) ;
#4869 = ORIENTED_EDGE ( 'NONE', *, *, #10897, .T. ) ;
#4870 = DIRECTION ( 'NONE',  ( 0.000000000000000000, 0.8191520442889952403, -0.5735764363510413855 ) ) ;
#4871 = DIRECTION ( 'NONE',  ( 3.469446951953612217E-16, -0.000000000000000000, 1.000000000000000000 ) ) ;
#4872 = CARTESIAN_POINT ( 'NONE',  ( 2.481649420246374138, 29.12180007765648426, -0.8687765177876252132 ) ) ;
#4873 = ORIENTED_EDGE ( 'NONE', *, *, #9442, .F. ) ;
#4874 = CARTESIAN_POINT ( 'NONE',  ( -3.481649420246370141, 32.87180007765647360, 1.193696214020542268 ) ) ;
#4875 = CARTESIAN_POINT ( 'NONE',  ( 4.000000000000000888, -24.43261708038802382, -10.61191331542860183 ) ) ;
#4876 = DIRECTION ( 'NONE',  ( -0.000000000000000000, -0.5735764363510414965, -0.8191520442889950182 ) ) ;
#4877 = CARTESIAN_POINT ( 'NONE',  ( 2.115076519116426024, 16.12819992234354416, 3.012182706137062294 ) ) ;
#4878 = EDGE_LOOP ( 'NONE', ( #12472, #9596, #7092, #1213 ) ) ;
#4879 = CARTESIAN_POINT ( 'NONE',  ( 2.121784821875004390, -19.42723073410004986, -9.870715949465248329 ) ) ;
#4880 = CARTESIAN_POINT ( 'NONE',  ( -1.027846397803541700, 17.49680007765647716, 3.346150245485522312 ) ) ;
#4881 = ORIENTED_EDGE ( 'NONE', *, *, #1404, .F. ) ;
#4882 = CYLINDRICAL_SURFACE ( 'NONE', #12503, 6.000000000000000888 ) ;
#4883 = DIRECTION ( 'NONE',  ( 1.000000000000000000, 0.000000000000000000, 0.000000000000000000 ) ) ;
#4884 = EDGE_CURVE ( 'NONE', #15656, #6744, #12847, .T. ) ;
#4885 = CARTESIAN_POINT ( 'NONE',  ( -4.243569643750000786, -26.22325101726895369, -13.16920360318992955 ) ) ;
#4886 = FACE_OUTER_BOUND ( 'NONE', #18364, .T. ) ;
#4887 = ADVANCED_FACE ( 'NONE', ( #3221 ), #15220, .T. ) ;
#4888 = CARTESIAN_POINT ( 'NONE',  ( 9.973478319601003506, -9.920655051887743880, 4.109042992078629553 ) ) ;
#4889 = CARTESIAN_POINT ( 'NONE',  ( 8.500000000000001776, 13.00000000000000178, -20.49999999999999645 ) ) ;
#4890 = CARTESIAN_POINT ( 'NONE',  ( 4.730628863548789710E-15, -15.82115571973984736, -6.856452161364834375 ) ) ;
#4891 = ORIENTED_EDGE ( 'NONE', *, *, #11809, .T. ) ;
#4892 = CARTESIAN_POINT ( 'NONE',  ( 8.000000000000005329, 38.59999999999999432, 2.499999999999997780 ) ) ;
#4893 = CARTESIAN_POINT ( 'NONE',  ( 4.713407268011036227E-15, -19.81026031600475790, -12.06313953008074868 ) ) ;
#4894 = ORIENTED_EDGE ( 'NONE', *, *, #14181, .T. ) ;
#4895 = VERTEX_POINT ( 'NONE', #5803 ) ;
#4896 = LINE ( 'NONE', #7670, #15763 ) ;
#4897 = CARTESIAN_POINT ( 'NONE',  ( 0.000000000000000000, 5.000000000000000000, 0.000000000000000000 ) ) ;
#4898 = CARTESIAN_POINT ( 'NONE',  ( -4.481649420246396787, 29.62819992234354416, -1.518615910253363399 ) ) ;
#4899 = LINE ( 'NONE', #15107, #14306 ) ;
#4900 = CARTESIAN_POINT ( 'NONE',  ( 1.497042530366522461, 21.12819992234354416, 2.161531897785029965 ) ) ;
#4901 = TOROIDAL_SURFACE ( 'NONE', #15276, 9.000000000000003553, 0.9999999999999991118 ) ;
#4902 = ORIENTED_EDGE ( 'NONE', *, *, #4707, .T. ) ;
#4903 = CARTESIAN_POINT ( 'NONE',  ( -4.481649420246366589, 20.37180007765648071, 1.518615910253458878 ) ) ;
#4904 = CARTESIAN_POINT ( 'NONE',  ( -1.999999999999996225, -19.12144277825430549, -9.066247182994150222 ) ) ;
#4905 = ORIENTED_EDGE ( 'NONE', *, *, #7189, .F. ) ;
#4906 = CARTESIAN_POINT ( 'NONE',  ( 0.000000000000000000, 5.000000000000000000, -2.499999999999999556 ) ) ;
#4907 = CARTESIAN_POINT ( 'NONE',  ( 2.864755990943265829, 39.49680007765647360, 2.011557305968487697 ) ) ;
#4908 = FACE_OUTER_BOUND ( 'NONE', #18193, .T. ) ;
#4909 = EDGE_CURVE ( 'NONE', #14839, #18119, #18355, .T. ) ;
#4910 = CARTESIAN_POINT ( 'NONE',  ( -5.330712181944246111E-15, -23.94572221871285578, -1.373575165951426369 ) ) ;
#4911 = EDGE_CURVE ( 'NONE', #11229, #6854, #17331, .T. ) ;
#4912 = AXIS2_PLACEMENT_3D ( 'NONE', #12531, #6690, #12344 ) ;
#4913 = CARTESIAN_POINT ( 'NONE',  ( 4.243569643750003451, -21.74275876667039853, -11.04188763791542804 ) ) ;
#4914 = CARTESIAN_POINT ( 'NONE',  ( 1.049162765915156337, -30.17532418831297747, -12.05880678485356583 ) ) ;
#4915 = ORIENTED_EDGE ( 'NONE', *, *, #1923, .F. ) ;
#4916 = VECTOR ( 'NONE', #9948, 1000.000000000000000 ) ;
#4917 = CARTESIAN_POINT ( 'NONE',  ( 6.097036691291187083, -11.55344374157293608, 15.47841750116241499 ) ) ;
#4918 = DIRECTION ( 'NONE',  ( -0.000000000000000000, 1.000000000000000000, -0.000000000000000000 ) ) ;
#4919 = FACE_BOUND ( 'NONE', #757, .T. ) ;
#4920 = CARTESIAN_POINT ( 'NONE',  ( 4.243569643749996345, -28.63886809700377611, -12.34757220902403851 ) ) ;
#4921 = VERTEX_POINT ( 'NONE', #15642 ) ;
#4922 = CARTESIAN_POINT ( 'NONE',  ( 3.500000000000000444, 30.75319992234354416, 0.05647727720529520379 ) ) ;
#4923 = LINE ( 'NONE', #9279, #10129 ) ;
#4924 = CARTESIAN_POINT ( 'NONE',  ( 4.730628863548789710E-15, -17.85376721605885209, -9.759322218313958075 ) ) ;
#4925 = CARTESIAN_POINT ( 'NONE',  ( -2.481649420246374138, 25.37180007765648426, 0.8687765177876256573 ) ) ;
#4926 = CARTESIAN_POINT ( 'NONE',  ( 3.673772985318163098, 15.50319992234354416, -2.599342558261029001 ) ) ;
#4927 = CARTESIAN_POINT ( 'NONE',  ( 2.121784821875004390, -23.81509047218551700, -16.13722908827605806 ) ) ;
#4928 = CARTESIAN_POINT ( 'NONE',  ( -1.999999999999996225, -23.76741191269774234, -15.70137874173500947 ) ) ;
#4929 =( BOUNDED_CURVE ( )  B_SPLINE_CURVE ( 2, ( #2850, #248, #14435, #64, #8856, #14342, #15555, #1373, #1640 ),
 .UNSPECIFIED., .F., .T. ) 
 B_SPLINE_CURVE_WITH_KNOTS ( ( 3, 2, 2, 2, 3 ),
 ( 0.5086206896551724865, 0.5114942528735632044, 0.5172413793103448620, 0.5229885057471264087, 0.5258620689655172376 ),
 .UNSPECIFIED. ) 
 CURVE ( )  GEOMETRIC_REPRESENTATION_ITEM ( )  RATIONAL_B_SPLINE_CURVE ( ( 0.9330127018922194093, 0.9330127018922206306, 1.000000000000000000, 0.8660254037844387076, 1.000000000000000000, 0.8660254037844387076, 1.000000000000000000, 0.9330127018922194093, 0.9330127018922194093 ) ) 
 REPRESENTATION_ITEM ( '' )  );
#4930 = CARTESIAN_POINT ( 'NONE',  ( -5.330712181944245322E-15, -25.78475166776338412, -3.999981407953017598 ) ) ;
#4931 = CARTESIAN_POINT ( 'NONE',  ( 1.444289557196047680, 39.74680007765648071, 4.262301884875704161 ) ) ;
#4932 = CARTESIAN_POINT ( 'NONE',  ( 0.000000000000000000, 40.79999999999999716, 2.500000000000000000 ) ) ;
#4933 = CARTESIAN_POINT ( 'NONE',  ( 4.000000000000003553, -25.03592396470017434, -15.49984274679136576 ) ) ;
#4934 = CARTESIAN_POINT ( 'NONE',  ( -9.000000000000003553, 29.79999999999999716, -2.500000000000001776 ) ) ;
#4935 = ORIENTED_EDGE ( 'NONE', *, *, #1986, .F. ) ;
#4936 = ORIENTED_EDGE ( 'NONE', *, *, #15856, .T. ) ;
#4937 =( NAMED_UNIT ( * ) SI_UNIT ( $, .STERADIAN. ) SOLID_ANGLE_UNIT ( ) );
#4938 = CARTESIAN_POINT ( 'NONE',  ( 9.000000000000001776, 29.79999999999999716, -2.500000000000002665 ) ) ;
#4939 = CARTESIAN_POINT ( 'NONE',  ( 7.082261791595104050, -12.11712549938399341, 11.44383700422758210 ) ) ;
#4940 = ORIENTED_EDGE ( 'NONE', *, *, #14901, .T. ) ;
#4941 = CARTESIAN_POINT ( 'NONE',  ( 1.989345975306457071, 31.00319992234355126, 1.515154207786300500 ) ) ;
#4942 = SURFACE_STYLE_FILL_AREA ( #11893 ) ;
#4943 = AXIS2_PLACEMENT_3D ( 'NONE', #2174, #10494, #16167 ) ;
#4944 = CARTESIAN_POINT ( 'NONE',  ( 4.243569643750000786, -26.06193264454523018, -12.93881709073364661 ) ) ;
#4945 = CARTESIAN_POINT ( 'NONE',  ( 1.027846397803542144, 23.74680007765647716, -3.346150245485522312 ) ) ;
#4946 = LINE ( 'NONE', #10601, #724 ) ;
#4947 = CARTESIAN_POINT ( 'NONE',  ( -1.998401444325281457E-14, -15.45745613286698550, -10.86990606519495195 ) ) ;
#4948 = CARTESIAN_POINT ( 'NONE',  ( 4.243569643749996345, -27.34832111521392761, -10.50448010937380161 ) ) ;
#4949 = EDGE_CURVE ( 'NONE', #1006, #13359, #15794, .T. ) ;
#4950 = EDGE_CURVE ( 'NONE', #17672, #5212, #8671, .T. ) ;
#4951 = AXIS2_PLACEMENT_3D ( 'NONE', #4889, #15936, #3233 ) ;
#4952 = CARTESIAN_POINT ( 'NONE',  ( 4.150834101209824212, -27.15734369766470380, -14.50322620280942587 ) ) ;
#4953 = EDGE_CURVE ( 'NONE', #244, #2141, #4929, .T. ) ;
#4954 = CYLINDRICAL_SURFACE ( 'NONE', #16901, 2.499999999999999556 ) ;
#4955 = EDGE_CURVE ( 'NONE', #2131, #12786, #8379, .T. ) ;
#4956 = DIRECTION ( 'NONE',  ( 1.000000000000000000, 0.000000000000000000, -4.336808689942021680E-16 ) ) ;
#4957 = CARTESIAN_POINT ( 'NONE',  ( 4.243569643749996345, -26.02551045887933867, -8.615310707232305631 ) ) ;
#4958 = DIRECTION ( 'NONE',  ( 0.000000000000000000, 0.000000000000000000, -1.000000000000000000 ) ) ;
#4959 = CARTESIAN_POINT ( 'NONE',  ( -2.000000000000005773, -22.45220093470416955, -1.744109083832446894 ) ) ;
#4960 = CARTESIAN_POINT ( 'NONE',  ( -1.497042530366477164, 27.62180007765648426, 2.161531897785062384 ) ) ;
#4961 = CYLINDRICAL_SURFACE ( 'NONE', #10904, 4.000000000000000000 ) ;
#4962 = CARTESIAN_POINT ( 'NONE',  ( 2.864755990943265829, 26.99680007765648071, 2.011557305968487697 ) ) ;
#4963 = DIRECTION ( 'NONE',  ( 0.000000000000000000, 0.000000000000000000, 1.000000000000000000 ) ) ;
#4964 =( NAMED_UNIT ( * ) PLANE_ANGLE_UNIT ( ) SI_UNIT ( $, .RADIAN. ) );
#4965 = VECTOR ( 'NONE', #5690, 1000.000000000000000 ) ;
#4966 = DIRECTION ( 'NONE',  ( -0.000000000000000000, 1.000000000000000000, -0.000000000000000000 ) ) ;
#4967 = VERTEX_POINT ( 'NONE', #4239 ) ;
#4968 = CARTESIAN_POINT ( 'NONE',  ( 2.121784821874994176, -25.27598940969881269, -5.409138659013170702 ) ) ;
#4969 = CARTESIAN_POINT ( 'NONE',  ( -1.135272562821090014, 15.99680007765647716, -3.311245368580554072 ) ) ;
#4970 = ORIENTED_EDGE ( 'NONE', *, *, #10207, .T. ) ;
#4971 = CARTESIAN_POINT ( 'NONE',  ( 4.336808689942017736E-16, 0.000000000000000000, 0.000000000000000000 ) ) ;
#4972 = FACE_OUTER_BOUND ( 'NONE', #6672, .T. ) ;
#4973 = EDGE_CURVE ( 'NONE', #14065, #17065, #7525, .T. ) ;
#4974 = CARTESIAN_POINT ( 'NONE',  ( -3.993033241984866866, -27.55172186255954259, -14.02642606169049522 ) ) ;
#4975 = CARTESIAN_POINT ( 'NONE',  ( 8.500000000000001776, 15.00000000000000178, -20.49999999999999645 ) ) ;
#4976 = COLOUR_RGB ( '',0.8941176470588234615, 0.8941176470588234615, 0.8941176470588234615 ) ;
#4977 = CARTESIAN_POINT ( 'NONE',  ( 6.804197231186874362, -11.93903049149238527, 12.87607830000603393 ) ) ;
#4978 = EDGE_CURVE ( 'NONE', #11611, #1200, #3951, .T. ) ;
#4980 = CARTESIAN_POINT ( 'NONE',  ( -1.071796769724496334, -24.10722040854632908, -3.173411524652919979 ) ) ;
#4979 = AXIS2_PLACEMENT_3D ( 'NONE', #6140, #15799, #311 ) ;
#4981 = CARTESIAN_POINT ( 'NONE',  ( -4.243569643750005227, -21.75595086079126261, -2.517747677556105845 ) ) ;
#4982 = ORIENTED_EDGE ( 'NONE', *, *, #8491, .F. ) ;
#4983 = DIRECTION ( 'NONE',  ( -0.000000000000000000, -0.5735764363510414965, -0.8191520442889950182 ) ) ;
#4984 = CARTESIAN_POINT ( 'NONE',  ( 4.713407268011036227E-15, -19.29404152328881850, -11.32590269022065499 ) ) ;
#4985 = VERTEX_POINT ( 'NONE', #13314 ) ;
#4986 = ORIENTED_EDGE ( 'NONE', *, *, #13858, .F. ) ;
#4987 = DIRECTION ( 'NONE',  ( -0.5000000000000061062, 0.000000000000000000, 0.8660254037844351549 ) ) ;
#4988 = FILL_AREA_STYLE ('',( #741 ) ) ;
#4989 = CARTESIAN_POINT ( 'NONE',  ( 2.733110507866328920, 36.12819992234354771, 3.862833514489095510 ) ) ;
#4990 = CARTESIAN_POINT ( 'NONE',  ( -2.798362969681409851, 32.25319992234354771, -2.102939460078765421 ) ) ;
#4991 = CARTESIAN_POINT ( 'NONE',  ( 2.518350579753611207, 20.62819992234354771, -0.7558219633769606149 ) ) ;
#4992 = VERTEX_POINT ( 'NONE', #12006 ) ;
#4993 = AXIS2_PLACEMENT_3D ( 'NONE', #11134, #10865, #11050 ) ;
#4994 = CARTESIAN_POINT ( 'NONE',  ( -3.673772985318163098, 39.25319992234354771, 2.599342558261029001 ) ) ;
#4995 = CIRCLE ( 'NONE', #16826, 0.9999999999999991118 ) ;
#4996 = CARTESIAN_POINT ( 'NONE',  ( 4.000000000000003553, -19.87373603754079809, -8.127474348190411035 ) ) ;
#4997 = EDGE_LOOP ( 'NONE', ( #8274, #5098, #11967, #6143 ) ) ;
#4998 = CYLINDRICAL_SURFACE ( 'NONE', #17481, 4.000000000000000000 ) ;
#4999 = CARTESIAN_POINT ( 'NONE',  ( -2.211161402132902243, 38.37180007765648071, -2.942372952327172886 ) ) ;
#5000 = CARTESIAN_POINT ( 'NONE',  ( 1.999999999999994449, -28.28117146841668728, -10.06874173291258856 ) ) ;
#5001 = CARTESIAN_POINT ( 'NONE',  ( -2.121784821874996396, -17.02896425960724969, -6.445636464281891520 ) ) ;
#5002 = CARTESIAN_POINT ( 'NONE',  ( -4.243569643750000786, -24.67459463912114259, -10.95749308360964136 ) ) ;
#5003 = PRODUCT_DEFINITION_SHAPE ( 'NONE', 'NONE',  #3009 ) ;
#5004 = TOROIDAL_SURFACE ( 'NONE', #16874, 9.000000000000001776, 0.9999999999999991118 ) ;
#5005 = CARTESIAN_POINT ( 'NONE',  ( 20.00000000000000355, 0.000000000000000000, 0.000000000000000000 ) ) ;
#5006 = ORIENTED_EDGE ( 'NONE', *, *, #3197, .F. ) ;
#5007 = CARTESIAN_POINT ( 'NONE',  ( -2.531783071939982754, -10.67720498481812541, 21.39218517664744823 ) ) ;
#5008 = SURFACE_SIDE_STYLE ('',( #3797 ) ) ;
#5009 = CARTESIAN_POINT ( 'NONE',  ( -4.243569643750000786, -26.99757920634285924, -14.27505886298007276 ) ) ;
#5010 = ORIENTED_EDGE ( 'NONE', *, *, #7443, .F. ) ;
#5011 = CARTESIAN_POINT ( 'NONE',  ( 0.05938372350920109732, 25.12819992234354416, -3.680117784833935701 ) ) ;
#5012 = CARTESIAN_POINT ( 'NONE',  ( 4.004198159875437923, -26.67562288373377299, -14.52967640179035413 ) ) ;
#5013 = CARTESIAN_POINT ( 'NONE',  ( -4.243569643750005227, -22.49801537532042062, -3.577525634854993086 ) ) ;
#5014 = CARTESIAN_POINT ( 'NONE',  ( 1.593127413382998903, 22.12180007765648071, 2.091722143975139669 ) ) ;
#5015 = ADVANCED_FACE ( 'NONE', ( #13214 ), #4690, .T. ) ;
#5016 = CARTESIAN_POINT ( 'NONE',  ( 4.481649420246397675, 15.87819992234354061, 1.518615910253363177 ) ) ;
#5017 = EDGE_CURVE ( 'NONE', #13681, #7716, #1832, .T. ) ;
#5018 = CARTESIAN_POINT ( 'NONE',  ( -4.000000000000004441, -27.65793290730917064, -11.19182377768135339 ) ) ;
#5019 = ORIENTED_EDGE ( 'NONE', *, *, #778, .F. ) ;
#5020 = EDGE_CURVE ( 'NONE', #10239, #6514, #12232, .T. ) ;
#5021 = AXIS2_PLACEMENT_3D ( 'NONE', #13500, #14829, #17712 ) ;
#5022 = CARTESIAN_POINT ( 'NONE',  ( -5.330712181944245322E-15, -24.75231408233150887, -2.525507728232826210 ) ) ;
#5023 = CARTESIAN_POINT ( 'NONE',  ( -2.115076519116362519, 17.62180007765647716, 3.012182706137107147 ) ) ;
#5024 = EDGE_CURVE ( 'NONE', #11442, #218, #2460, .T. ) ;
#5025 = CARTESIAN_POINT ( 'NONE',  ( 20.00000000000000355, 0.000000000000000000, 3.309499999999999886 ) ) ;
#5026 = FACE_OUTER_BOUND ( 'NONE', #8859, .T. ) ;
#5027 = LINE ( 'NONE', #16353, #17751 ) ;
#5028 = ORIENTED_EDGE ( 'NONE', *, *, #8853, .F. ) ;
#5029 = VERTEX_POINT ( 'NONE', #436 ) ;
#5030 = DIRECTION ( 'NONE',  ( 0.000000000000000000, 1.000000000000000000, 0.000000000000000000 ) ) ;
#5031 = DIRECTION ( 'NONE',  ( -0.000000000000000000, -1.000000000000000000, -0.000000000000000000 ) ) ;
#5032 = CARTESIAN_POINT ( 'NONE',  ( 0.000000000000000000, 3.000000000000000000, 0.000000000000000000 ) ) ;
#5033 = VERTEX_POINT ( 'NONE', #1935 ) ;
#5034 = TOROIDAL_SURFACE ( 'NONE', #16003, 9.000000000000001776, 0.9999999999999991118 ) ;
#5035 = CARTESIAN_POINT ( 'NONE',  ( -1.593127413382952939, 26.62819992234354416, 2.091722143975172532 ) ) ;
#5036 = CARTESIAN_POINT ( 'NONE',  ( -2.121784821874996396, -22.96548037584052793, -14.92386012267298945 ) ) ;
#5037 = CARTESIAN_POINT ( 'NONE',  ( -0.05938372350927861171, 26.12180007765647005, -3.680117784833935701 ) ) ;
#5038 =( BOUNDED_CURVE ( )  B_SPLINE_CURVE ( 3, ( #11201, #937, #1306, #2428 ),
 .UNSPECIFIED., .F., .T. ) 
 B_SPLINE_CURVE_WITH_KNOTS ( ( 4, 4 ),
 ( 0.000000000000000000, 1.029696800837750059 ),
 .UNSPECIFIED. ) 
 CURVE ( )  GEOMETRIC_REPRESENTATION_ITEM ( )  RATIONAL_B_SPLINE_CURVE ( ( 1.000000000000000000, 0.9135782535825738293, 0.9135782535825738293, 1.000000000000000000 ) ) 
 REPRESENTATION_ITEM ( '' )  );
#5039 = FACE_OUTER_BOUND ( 'NONE', #6195, .T. ) ;
#5040 = CARTESIAN_POINT ( 'NONE',  ( -1.661723472263481630E-14, -21.80128239342201724, -13.82776510965112671 ) ) ;
#5041 = CARTESIAN_POINT ( 'NONE',  ( -4.243569643750005227, -26.91813878795063886, -9.890116076157061897 ) ) ;
#5042 = AXIS2_PLACEMENT_3D ( 'NONE', #8352, #16445, #16815 ) ;
#5043 = DIRECTION ( 'NONE',  ( 0.000000000000000000, 0.9936001553129348851, 0.1129545544106647231 ) ) ;
#5044 = CARTESIAN_POINT ( 'NONE',  ( -1.071796769724496334, -23.39741956926685518, -2.159710870852054931 ) ) ;
#5045 = CARTESIAN_POINT ( 'NONE',  ( -1.734723475976807094E-15, 43.00000000000000000, -11.50000000000000178 ) ) ;
#5046 = CARTESIAN_POINT ( 'NONE',  ( -4.243569643750000786, -23.35178398278655010, -9.068323681468148934 ) ) ;
#5047 = VERTEX_POINT ( 'NONE', #3492 ) ;
#5048 = FACE_OUTER_BOUND ( 'NONE', #15426, .T. ) ;
#5049 = CARTESIAN_POINT ( 'NONE',  ( 3.064181913176683203, -21.66367673124435100, -2.174801284911689780 ) ) ;
#5050 = CARTESIAN_POINT ( 'NONE',  ( -2.500000000000001332, 32.99680007765648071, 0.05647727720535858364 ) ) ;
#5051 = VERTEX_POINT ( 'NONE', #13406 ) ;
#5052 = CARTESIAN_POINT ( 'NONE',  ( 3.518350579753631191, 31.87180007765647716, 1.080741659609802729 ) ) ;
#5053 = CARTESIAN_POINT ( 'NONE',  ( 1.475796370471763337E-14, -22.05939178977998694, -14.19638352958117267 ) ) ;
#5054 = APPLICATION_PROTOCOL_DEFINITION ( 'draft international standard', 'automotive_design', 1998, #630 ) ;
#5055 = AXIS2_PLACEMENT_3D ( 'NONE', #14496, #10020, #7239 ) ;
#5056 = CIRCLE ( 'NONE', #2417, 2.499999999999999556 ) ;
#5057 = DIRECTION ( 'NONE',  ( 1.028113302204111856E-14, -0.1129545544106654864, 0.9936001553129347741 ) ) ;
#5058 = ORIENTED_EDGE ( 'NONE', *, *, #6349, .T. ) ;
#5059 = CARTESIAN_POINT ( 'NONE',  ( -5.330712181944246111E-15, -26.55907985683728967, -5.105836667743160362 ) ) ;
#5060 = CARTESIAN_POINT ( 'NONE',  ( -3.500000000000000444, 20.49680007765647716, 0.05647727720536892260 ) ) ;
#5061 = ORIENTED_EDGE ( 'NONE', *, *, #1321, .F. ) ;
#5062 = EDGE_CURVE ( 'NONE', #5212, #13188, #628, .T. ) ;
#5063 = FACE_OUTER_BOUND ( 'NONE', #7850, .T. ) ;
#5064 = PLANE ( 'NONE',  #2929 ) ;
#5065 = CARTESIAN_POINT ( 'NONE',  ( -1.355220984792064876, -23.95640476330365587, -16.63505457156503908 ) ) ;
#5066 = AXIS2_PLACEMENT_3D ( 'NONE', #14716, #6259, #5140 ) ;
#5067 = CARTESIAN_POINT ( 'NONE',  ( 5.992170350750239294, -10.31447287898148168, 0.09153525861095850036 ) ) ;
#5068 = CARTESIAN_POINT ( 'NONE',  ( -1.999999999999996225, -18.08900519282243025, -7.591773503273958390 ) ) ;
#5069 = CARTESIAN_POINT ( 'NONE',  ( 4.243569643750003451, -18.64544601037477278, -6.618466598754856101 ) ) ;
#5070 = ORIENTED_EDGE ( 'NONE', *, *, #17401, .T. ) ;
#5071 = CARTESIAN_POINT ( 'NONE',  ( 9.000000000000005329, 38.59999999999999432, 2.499999999999997335 ) ) ;
#5072 = CARTESIAN_POINT ( 'NONE',  ( -2.000000000000005773, -26.58195127643166700, -7.642003802713210447 ) ) ;
#5073 = CARTESIAN_POINT ( 'NONE',  ( -2.115076519116362519, 35.12180007765645939, 3.012182706137107147 ) ) ;
#5074 = ORIENTED_EDGE ( 'NONE', *, *, #14025, .F. ) ;
#5075 = ORIENTED_EDGE ( 'NONE', *, *, #12780, .F. ) ;
#5076 = CARTESIAN_POINT ( 'NONE',  ( -3.999999999999997335, -19.52959017573017064, -7.635983121617017311 ) ) ;
#5077 = CARTESIAN_POINT ( 'NONE',  ( -2.829195390882724315, 34.12819992234354771, 3.793023760679264722 ) ) ;
#5078 = CARTESIAN_POINT ( 'NONE',  ( -1.027846397803611866, 37.50319992234354061, -3.346150245485499219 ) ) ;
#5079 = CARTESIAN_POINT ( 'NONE',  ( 0.7188294034286553114, 28.75319992234354771, 2.395093729190349130 ) ) ;
#5080 = VERTEX_POINT ( 'NONE', #11826 ) ;
#5081 = CARTESIAN_POINT ( 'NONE',  ( 2.829195390882805583, 19.62180007765647716, 3.793023760679204770 ) ) ;
#5082 = ADVANCED_FACE ( 'NONE', ( #3583 ), #7469, .T. ) ;
#5083 = CARTESIAN_POINT ( 'NONE',  ( 2.000000000000004441, -17.61580463283282683, -6.915973066735536356 ) ) ;
#5084 = ORIENTED_EDGE ( 'NONE', *, *, #12488, .F. ) ;
#5085 = FACE_OUTER_BOUND ( 'NONE', #8902, .T. ) ;
#5086 = CARTESIAN_POINT ( 'NONE',  ( -2.115076519116362519, 37.62180007765648071, 3.012182706137107147 ) ) ;
#5087 = CARTESIAN_POINT ( 'NONE',  ( 4.000000000000003553, -21.93861120840455214, -11.07642170763079292 ) ) ;
#5088 = AXIS2_PLACEMENT_3D ( 'NONE', #6027, #7228, #7414 ) ;
#5089 = CARTESIAN_POINT ( 'NONE',  ( -4.243569643750000786, -20.77069001920686375, -5.382139482167671574 ) ) ;
#5090 = AXIS2_PLACEMENT_3D ( 'NONE', #17657, #17373, #9183 ) ;
#5091 = CARTESIAN_POINT ( 'NONE',  ( -2.121784821874996396, -21.70719706859543408, -13.12684532551400629 ) ) ;
#5092 = AXIS2_PLACEMENT_3D ( 'NONE', #152, #10242, #17136 ) ;
#5093 = CARTESIAN_POINT ( 'NONE',  ( -1.373763480980777274, -30.12088136896208113, -12.14767278240311654 ) ) ;
#5094 = ORIENTED_EDGE ( 'NONE', *, *, #10488, .F. ) ;
#5095 = CARTESIAN_POINT ( 'NONE',  ( -7.971931588564060256, -10.00000000000000178, 17.73270869615951639 ) ) ;
#5096 =( LENGTH_UNIT ( ) NAMED_UNIT ( * ) SI_UNIT ( .MILLI., .METRE. ) );
#5097 = CARTESIAN_POINT ( 'NONE',  ( -4.243569643750005227, -28.46679516609844995, -12.10182659573734476 ) ) ;
#5098 = ORIENTED_EDGE ( 'NONE', *, *, #12016, .F. ) ;
#5099 = CARTESIAN_POINT ( 'NONE',  ( 1.027846397803612311, 38.75319992234354061, 3.346150245485499219 ) ) ;
#5100 = CARTESIAN_POINT ( 'NONE',  ( 3.511779744724054186, -25.38768362883276097, -15.39278514861212699 ) ) ;
#5101 = CARTESIAN_POINT ( 'NONE',  ( 2.121784821874994176, -22.66263177157437525, -1.676877157221437376 ) ) ;
#5102 = CARTESIAN_POINT ( 'NONE',  ( 0.05938372350926800214, 32.37180007765648782, 2.628655560595669183 ) ) ;
#5103 = CIRCLE ( 'NONE', #2166, 0.9999999999999991118 ) ;
#5104 = CARTESIAN_POINT ( 'NONE',  ( -0.05938372350920063936, 38.87819992234354771, 3.680117784833935701 ) ) ;
#5105 = AXIS2_PLACEMENT_3D ( 'NONE', #7298, #10546, #8980 ) ;
#5106 = CARTESIAN_POINT ( 'NONE',  ( -4.000000000000004441, -26.88360471823526865, -10.08596851789121018 ) ) ;
#5107 = ORIENTED_EDGE ( 'NONE', *, *, #2006, .T. ) ;
#5108 = APPLICATION_CONTEXT ( 'automotive_design' ) ;
#5109 = CARTESIAN_POINT ( 'NONE',  ( 4.243569643750000786, -21.70633658100450702, -6.718381254414091508 ) ) ;
#5110 = CARTESIAN_POINT ( 'NONE',  ( -3.607379964056306676, 40.24680007765648071, 2.690724712371306282 ) ) ;
#5111 = DIRECTION ( 'NONE',  ( -1.000000000000000000, -0.000000000000000000, -0.000000000000000000 ) ) ;
#5112 = ADVANCED_FACE ( 'NONE', ( #17522 ), #3371, .T. ) ;
#5113 = VECTOR ( 'NONE', #3674, 1000.000000000000000 ) ;
#5114 = AXIS2_PLACEMENT_3D ( 'NONE', #16334, #3624, #16243 ) ;
#5115 = EDGE_CURVE ( 'NONE', #13628, #10626, #11061, .T. ) ;
#5116 = DIRECTION ( 'NONE',  ( -0.000000000000000000, -0.000000000000000000, -1.000000000000000000 ) ) ;
#5117 = EDGE_LOOP ( 'NONE', ( #6504, #7510, #6578, #4186 ) ) ;
#5118 = ORIENTED_EDGE ( 'NONE', *, *, #444, .F. ) ;
#5119 = CARTESIAN_POINT ( 'NONE',  ( -1.027846397803541700, 17.49680007765647716, 3.346150245485522312 ) ) ;
#5120 = DIRECTION ( 'NONE',  ( -1.000000000000000000, 0.000000000000000000, 0.000000000000000000 ) ) ;
#5121 = CARTESIAN_POINT ( 'NONE',  ( -1.661723472263481630E-14, -20.76884480799014554, -12.35329142993093576 ) ) ;
#5122 = VERTEX_POINT ( 'NONE', #17701 ) ;
#5123 = CARTESIAN_POINT ( 'NONE',  ( 2.518350579753611207, 35.62819992234354771, -0.7558219633769606149 ) ) ;
#5124 = CARTESIAN_POINT ( 'NONE',  ( -4.243569643750005227, -25.85343752797401606, -8.369565093945613654 ) ) ;
#5125 = CARTESIAN_POINT ( 'NONE',  ( -2.115076519116362519, 22.62180007765647360, 3.012182706137107147 ) ) ;
#5126 = EDGE_CURVE ( 'NONE', #2406, #6613, #16107, .T. ) ;
#5127 = CARTESIAN_POINT ( 'NONE',  ( -4.000000000000003553, 6.938893903907228378E-15, 24.28148006742132026 ) ) ;
#5128 = CARTESIAN_POINT ( 'NONE',  ( -1.071796769724496334, -20.75731810727131332, -12.33682959527501488 ) ) ;
#5129 = CIRCLE ( 'NONE', #13672, 0.4000000000000001887 ) ;
#5130 = CIRCLE ( 'NONE', #7196, 8.000000000000001776 ) ;
#5131 = CARTESIAN_POINT ( 'NONE',  ( 4.730628863548789710E-15, -20.98334364689921827, -14.22882055996578643 ) ) ;
#5132 = CARTESIAN_POINT ( 'NONE',  ( 0.3999999999999975797, 7.470345474798854293E-16, -6.099999999999999645 ) ) ;
#5133 = CARTESIAN_POINT ( 'NONE',  ( 4.481649420246366589, 26.62180007765648426, -1.518615910253458212 ) ) ;
#5134 = DIRECTION ( 'NONE',  ( -0.000000000000000000, 1.000000000000000000, -0.000000000000000000 ) ) ;
#5135 = EDGE_CURVE ( 'NONE', #11008, #9284, #7746, .T. ) ;
#5136 = LINE ( 'NONE', #13760, #1131 ) ;
#5137 =( BOUNDED_CURVE ( )  B_SPLINE_CURVE ( 2, ( #1594, #11677, #4550, #12886, #4636, #15774, #1502, #7513, #3074 ),
 .UNSPECIFIED., .F., .F. ) 
 B_SPLINE_CURVE_WITH_KNOTS ( ( 3, 2, 2, 2, 3 ),
 ( 0.5258620689655172376, 0.5287356321839080664, 0.5344827586206896131, 0.5402298850574712707, 0.5431034482758620996 ),
 .UNSPECIFIED. ) 
 CURVE ( )  GEOMETRIC_REPRESENTATION_ITEM ( )  RATIONAL_B_SPLINE_CURVE ( ( 0.9330127018922194093, 0.9330127018922194093, 1.000000000000000000, 0.8660254037844387076, 1.000000000000000000, 0.8660254037844387076, 1.000000000000000000, 0.9330127018922194093, 0.9330127018922194093 ) ) 
 REPRESENTATION_ITEM ( '' )  );
#5138 = CARTESIAN_POINT ( 'NONE',  ( -4.243569643750005227, -23.78856235711026912, -5.420617734505229990 ) ) ;
#5139 = ORIENTED_EDGE ( 'NONE', *, *, #141, .T. ) ;
#5140 = DIRECTION ( 'NONE',  ( 0.000000000000000000, 0.000000000000000000, -1.000000000000000000 ) ) ;
#5141 = CARTESIAN_POINT ( 'NONE',  ( 1.300000000000000044, 0.7216878364870329410, 1.249999999999999778 ) ) ;
#5142 = CYLINDRICAL_SURFACE ( 'NONE', #7011, 0.9999999999999991118 ) ;
#5143 = CARTESIAN_POINT ( 'NONE',  ( -0.05938372350926768989, 33.62180007765647360, -2.628655560595669183 ) ) ;
#5144 = CARTESIAN_POINT ( 'NONE',  ( 1.999999999999994449, -23.37709293761528784, -3.064991754241682465 ) ) ;
#5145 = CARTESIAN_POINT ( 'NONE',  ( 1.135272562821090458, 29.74680007765647716, 3.311245368580554072 ) ) ;
#5146 = CARTESIAN_POINT ( 'NONE',  ( -1.999999999999996225, -17.31467700374852470, -6.485918243483816958 ) ) ;
#5147 = ITEM_DEFINED_TRANSFORMATION ( 'NONE', 'NONE', #15182,  #16940 ) ;
#5148 = DIRECTION ( 'NONE',  ( 0.000000000000000000, 0.000000000000000000, 1.000000000000000000 ) ) ;
#5149 = PRODUCT_DEFINITION_CONTEXT ( 'detailed design', #7837, 'design' ) ;
#5150 = ORIENTED_EDGE ( 'NONE', *, *, #2081, .T. ) ;
#5151 = CARTESIAN_POINT ( 'NONE',  ( 4.243569643749997233, -23.47668016984440342, -4.975203810423082906 ) ) ;
#5152 = CARTESIAN_POINT ( 'NONE',  ( 2.798362969681366330, 26.49680007765648071, -2.102939460078824929 ) ) ;
#5153 = ORIENTED_EDGE ( 'NONE', *, *, #1859, .F. ) ;
#5154 = AXIS2_PLACEMENT_3D ( 'NONE', #3809, #8260, #9465 ) ;
#5155 = PRODUCT_DEFINITION_SHAPE ( 'NONE', 'NONE',  #18371 ) ;
#5156 = CARTESIAN_POINT ( 'NONE',  ( -8.000000000000001776, 20.99999999999999289, 2.499999999999995115 ) ) ;
#5157 = EDGE_CURVE ( 'NONE', #2835, #4535, #5726, .T. ) ;
#5158 = DIRECTION ( 'NONE',  ( 0.000000000000000000, 0.000000000000000000, 1.000000000000000000 ) ) ;
#5159 = DIRECTION ( 'NONE',  ( 0.000000000000000000, -0.000000000000000000, 1.000000000000000000 ) ) ;
#5160 = CARTESIAN_POINT ( 'NONE',  ( 9.828195458270586826, -9.943122604294416078, 1.729283279605983159 ) ) ;
#5161 = DIRECTION ( 'NONE',  ( -3.373073425510457965E-16, 0.000000000000000000, -1.000000000000000000 ) ) ;
#5162 = CARTESIAN_POINT ( 'NONE',  ( -5.330712181944245322E-15, -24.49420468597353562, -2.156889308302778030 ) ) ;
#5163 = ORIENTED_EDGE ( 'NONE', *, *, #1859, .T. ) ;
#5164 = CARTESIAN_POINT ( 'NONE',  ( 0.000000000000000000, 43.00000000000000000, 2.500000000000000000 ) ) ;
#5165 = CARTESIAN_POINT ( 'NONE',  ( 4.000000000000003553, -21.74502916184101764, -10.79995789369002246 ) ) ;
#5166 = CARTESIAN_POINT ( 'NONE',  ( -2.211161402132902243, 33.37180007765648071, -2.942372952327172886 ) ) ;
#5167 = ORIENTED_EDGE ( 'NONE', *, *, #15350, .T. ) ;
#5168 = ORIENTED_EDGE ( 'NONE', *, *, #4144, .T. ) ;
#5169 = LINE ( 'NONE', #18175, #12206 ) ;
#5170 = CARTESIAN_POINT ( 'NONE',  ( 3.673772985318163098, 33.00319992234354771, -2.599342558261029001 ) ) ;
#5171 = DIRECTION ( 'NONE',  ( -1.000000000000000000, 0.000000000000000000, 4.336808689942021680E-16 ) ) ;
#5172 = CARTESIAN_POINT ( 'NONE',  ( 1.593127413382953383, 30.37819992234354061, -2.091722143975172532 ) ) ;
#5173 = ORIENTED_EDGE ( 'NONE', *, *, #6036, .T. ) ;
#5174 = CARTESIAN_POINT ( 'NONE',  ( 1.336863392178479160, 26.24680007765647716, -4.297206761780677731 ) ) ;
#5175 = CARTESIAN_POINT ( 'NONE',  ( 4.000000000000000888, -20.23833938886609118, -4.621863990558560786 ) ) ;
#5176 = ORIENTED_EDGE ( 'NONE', *, *, #660, .F. ) ;
#5177 = PLANE ( 'NONE',  #6796 ) ;
#5178 = ADVANCED_BREP_SHAPE_REPRESENTATION ( '', ( #1586, #16940 ), #340 ) ;
#5179 = CARTESIAN_POINT ( 'NONE',  ( -2.115076519116362519, 40.12180007765648071, 3.012182706137107147 ) ) ;
#5180 = CARTESIAN_POINT ( 'NONE',  ( 15.00000000000000355, 10.00000000000000000, 30.00000000000000000 ) ) ;
#5181 = EDGE_CURVE ( 'NONE', #11177, #2342, #10621, .T. ) ;
#5182 = CARTESIAN_POINT ( 'NONE',  ( -4.243569643750000786, -19.99636183013295820, -4.276284222377527477 ) ) ;
#5183 = CARTESIAN_POINT ( 'NONE',  ( -4.243569643750005227, -25.62759180616079746, -8.047023976506819665 ) ) ;
#5184 = EDGE_CURVE ( 'NONE', #13, #646, #14632, .T. ) ;
#5185 = DIRECTION ( 'NONE',  ( 0.000000000000000000, 0.8191520442889952403, -0.5735764363510413855 ) ) ;
#5186 = EDGE_CURVE ( 'NONE', #13000, #6995, #14926, .T. ) ;
#5187 = ORIENTED_EDGE ( 'NONE', *, *, #17953, .F. ) ;
#5188 = PRODUCT_DEFINITION_CONTEXT ( 'detailed design', #14235, 'design' ) ;
#5189 = FACE_OUTER_BOUND ( 'NONE', #13823, .T. ) ;
#5190 = CARTESIAN_POINT ( 'NONE',  ( -8.500000000000005329, 10.00000000000000000, 18.49999999999999645 ) ) ;
#5191 = CARTESIAN_POINT ( 'NONE',  ( -1.734723475976807094E-15, 18.79999999999999361, -12.50000000000000000 ) ) ;
#5192 = CARTESIAN_POINT ( 'NONE',  ( -2.121784821874996396, -23.25585344674324162, -15.33855584509429271 ) ) ;
#5193 = ORIENTED_EDGE ( 'NONE', *, *, #9036, .F. ) ;
#5194 = CARTESIAN_POINT ( 'NONE',  ( 2.115076519116426024, 36.12819992234355482, 3.012182706137062294 ) ) ;
#5195 = ADVANCED_FACE ( 'NONE', ( #3758 ), #8110, .T. ) ;
#5196 = CARTESIAN_POINT ( 'NONE',  ( -1.734723475976807094E-15, 20.99999999999999289, -2.500000000000000000 ) ) ;
#5197 = CARTESIAN_POINT ( 'NONE',  ( 4.243569643749996345, -22.15386951350980738, -3.086034408281590036 ) ) ;
#5198 = CARTESIAN_POINT ( 'NONE',  ( -1.989345975306426206, 32.74680007765648071, 1.515154207786343799 ) ) ;
#5199 = SHAPE_REPRESENTATION ( 'Return Spring', ( #16940 ), #6566 ) ;
#5200 = CARTESIAN_POINT ( 'NONE',  ( 1.336863392178569754, 26.25319992234354416, 4.297206761780648421 ) ) ;
#5201 = CARTESIAN_POINT ( 'NONE',  ( 3.999999999999996447, -26.53945885642465186, -9.594477291317808465 ) ) ;
#5202 = ORIENTED_EDGE ( 'NONE', *, *, #5184, .T. ) ;
#5203 = VECTOR ( 'NONE', #811, 1000.000000000000114 ) ;
#5204 = CARTESIAN_POINT ( 'NONE',  ( -4.243569643750005227, -22.53027904986517527, -3.623602937346249497 ) ) ;
#5205 = CARTESIAN_POINT ( 'NONE',  ( -3.607379964056306676, 37.74680007765647360, 2.690724712371306282 ) ) ;
#5206 =( NAMED_UNIT ( * ) PLANE_ANGLE_UNIT ( ) SI_UNIT ( $, .RADIAN. ) );
#5207 = CARTESIAN_POINT ( 'NONE',  ( -2.121784821874996396, -21.15871460133474713, -12.34353118316265707 ) ) ;
#5208 = VECTOR ( 'NONE', #13137, 1000.000000000000000 ) ;
#5209 = FACE_OUTER_BOUND ( 'NONE', #10320, .T. ) ;
#5210 = LINE ( 'NONE', #7987, #7634 ) ;
#5211 = ORIENTED_EDGE ( 'NONE', *, *, #7275, .F. ) ;
#5212 = VERTEX_POINT ( 'NONE', #9678 ) ;
#5213 = CARTESIAN_POINT ( 'NONE',  ( 2.864755990943265829, 19.49680007765648071, 2.011557305968487697 ) ) ;
#5214 = CARTESIAN_POINT ( 'NONE',  ( 6.808477104226121845, -11.94136413928387519, 12.86032843472113818 ) ) ;
#5215 = ORIENTED_EDGE ( 'NONE', *, *, #16997, .F. ) ;
#5216 = CARTESIAN_POINT ( 'NONE',  ( 0.05938372350920109732, 15.12819992234354238, -3.680117784833935701 ) ) ;
#5217 = SURFACE_STYLE_USAGE ( .BOTH. , #14175 ) ;
#5218 = CARTESIAN_POINT ( 'NONE',  ( -4.243569643750000786, -23.60989337914451625, -9.436942101398194893 ) ) ;
#5219 = CARTESIAN_POINT ( 'NONE',  ( 2.798362969681366330, 31.49680007765647716, -2.102939460078824929 ) ) ;
#5220 = CARTESIAN_POINT ( 'NONE',  ( 2.115076519116426024, 21.12819992234353705, 3.012182706137062294 ) ) ;
#5221 = LINE ( 'NONE', #9481, #3387 ) ;
#5222 = AXIS2_PLACEMENT_3D ( 'NONE', #139, #9955, #12836 ) ;
#5223 = CARTESIAN_POINT ( 'NONE',  ( 8.500000000000019540, 10.00000000000000000, 18.49999999999998934 ) ) ;
#5224 = CARTESIAN_POINT ( 'NONE',  ( -4.243569643750005227, -26.14381059887672976, -8.784260816366916913 ) ) ;
#5225 = ADVANCED_FACE ( 'NONE', ( #9320 ), #2491, .T. ) ;
#5226 = FACE_OUTER_BOUND ( 'NONE', #5366, .T. ) ;
#5227 = CARTESIAN_POINT ( 'NONE',  ( -0.05938372350928957516, 23.62180007765647005, -4.731580009072201776 ) ) ;
#5228 = LINE ( 'NONE', #16563, #2617 ) ;
#5229 = CIRCLE ( 'NONE', #8192, 0.4999999999999992784 ) ;
#5230 = CARTESIAN_POINT ( 'NONE',  ( 4.243569643750000786, -21.93218230281772918, -7.040922371852881945 ) ) ;
#5231 = EDGE_LOOP ( 'NONE', ( #1657, #11566, #1971, #11980, #9172 ) ) ;
#5232 = DIRECTION ( 'NONE',  ( 0.000000000000000000, -0.000000000000000000, -1.000000000000000000 ) ) ;
#5233 = CARTESIAN_POINT ( 'NONE',  ( 1.071796769724485232, -28.53655409498856699, -9.499155600141175881 ) ) ;
#5234 = CARTESIAN_POINT ( 'NONE',  ( 1.593127413382998903, 34.62180007765648071, 2.091722143975139669 ) ) ;
#5235 = CARTESIAN_POINT ( 'NONE',  ( 4.299564228933482956E-15, -17.15531325897858039, -7.192633550910265683 ) ) ;
#5236 = CARTESIAN_POINT ( 'NONE',  ( -2.798362969681365886, 37.74680007765647360, 2.102939460078824929 ) ) ;
#5237 = DIRECTION ( 'NONE',  ( 3.469446951953612217E-16, -0.000000000000000000, 1.000000000000000000 ) ) ;
#5238 = APPLICATION_PROTOCOL_DEFINITION ( 'draft international standard', 'automotive_design', 1998, #4758 ) ;
#5239 = CARTESIAN_POINT ( 'NONE',  ( -2.908635224650709894, 15.00000000000001066, -2.619577396687581050 ) ) ;
#5240 = ADVANCED_FACE ( 'NONE', ( #14995 ), #13769, .F. ) ;
#5241 = ORIENTED_EDGE ( 'NONE', *, *, #10788, .T. ) ;
#5242 = CARTESIAN_POINT ( 'NONE',  ( 2.121784821875004390, -17.87857435595223876, -7.659005429884962801 ) ) ;
#5243 = CARTESIAN_POINT ( 'NONE',  ( 3.481649420246369697, 21.62180007765647360, -1.193696214020541824 ) ) ;
#5244 = ADVANCED_FACE ( 'NONE', ( #8020 ), #10805, .T. ) ;
#5245 = AXIS2_PLACEMENT_3D ( 'NONE', #5344, #5161, #6822 ) ;
#5246 = ORIENTED_EDGE ( 'NONE', *, *, #2025, .T. ) ;
#5247 = EDGE_CURVE ( 'NONE', #12052, #2259, #1082, .T. ) ;
#5248 = CARTESIAN_POINT ( 'NONE',  ( -3.706921591972381904E-14, -18.44586024076842534, -9.035725650560502586 ) ) ;
#5249 = DIRECTION ( 'NONE',  ( 0.000000000000000000, 0.000000000000000000, 1.000000000000000000 ) ) ;
#5250 = PLANE ( 'NONE',  #13204 ) ;
#5251 = DIRECTION ( 'NONE',  ( 0.000000000000000000, -1.502314598737159031E-16, -1.000000000000000000 ) ) ;
#5252 = CARTESIAN_POINT ( 'NONE',  ( -8.000000000000001776, 46.00000000000000000, -2.500000000000000888 ) ) ;
#5253 = CARTESIAN_POINT ( 'NONE',  ( -4.243569643750005227, -27.66020330247980041, -10.94989403345594425 ) ) ;
#5254 = ORIENTED_EDGE ( 'NONE', *, *, #11755, .T. ) ;
#5255 = DIRECTION ( 'NONE',  ( -1.000000000000000000, 0.000000000000000000, 4.336808689942021680E-16 ) ) ;
#5256 = CARTESIAN_POINT ( 'NONE',  ( -3.999999999999997335, -19.33600812916663614, -7.359519307676247735 ) ) ;
#5257 = AXIS2_PLACEMENT_3D ( 'NONE', #13233, #6712, #550 ) ;
#5258 = CARTESIAN_POINT ( 'NONE',  ( -0.7188294034286043521, 17.49680007765647716, 2.395093729190366005 ) ) ;
#5259 = EDGE_LOOP ( 'NONE', ( #8572, #1053, #8322, #8785 ) ) ;
#5260 = CIRCLE ( 'NONE', #9695, 2.149999999999999023 ) ;
#5261 = ORIENTED_EDGE ( 'NONE', *, *, #8082, .F. ) ;
#5262 = CARTESIAN_POINT ( 'NONE',  ( -1.071796769724496334, -24.36532980490429878, -3.542029944582967271 ) ) ;
#5263 = SURFACE_STYLE_FILL_AREA ( #9519 ) ;
#5264 = CARTESIAN_POINT ( 'NONE',  ( -3.607379964056363075, 37.25319992234354061, -2.690724712371229899 ) ) ;
#5265 = CARTESIAN_POINT ( 'NONE',  ( -5.577813053751546416E-15, -29.32240898478130120, -10.62147269458723464 ) ) ;
#5266 = CARTESIAN_POINT ( 'NONE',  ( -2.055738996568281518, 24.25319992234354061, 1.423772053676066962 ) ) ;
#5267 = ORIENTED_EDGE ( 'NONE', *, *, #14835, .T. ) ;
#5268 = CARTESIAN_POINT ( 'NONE',  ( -2.121784821874996396, -22.99774405038527547, -14.96993742516424497 ) ) ;
#5269 = CARTESIAN_POINT ( 'NONE',  ( 4.518350579753633411, 26.87180007765647716, 1.405661355842698468 ) ) ;
#5270 = CARTESIAN_POINT ( 'NONE',  ( -4.000000000000000888, -20.10928469068709745, -4.437554780593541359 ) ) ;
#5271 = VERTEX_POINT ( 'NONE', #16573 ) ;
#5272 = CARTESIAN_POINT ( 'NONE',  ( -3.706921591972381904E-14, -18.44586024076842534, -9.035725650560502586 ) ) ;
#5273 = VECTOR ( 'NONE', #17389, 1000.000000000000000 ) ;
#5274 = DIRECTION ( 'NONE',  ( -3.373073425510457965E-16, 0.000000000000000000, -1.000000000000000000 ) ) ;
#5275 = ADVANCED_FACE ( 'NONE', ( #994 ), #15175, .F. ) ;
#5276 = CARTESIAN_POINT ( 'NONE',  ( 4.243569643750000786, -20.12541652831194838, -4.460593432342547793 ) ) ;
#5277 = CARTESIAN_POINT ( 'NONE',  ( -5.330712181944245322E-15, -26.81718925319525937, -5.474455087673208986 ) ) ;
#5278 = DIRECTION ( 'NONE',  ( 0.000000000000000000, 0.000000000000000000, 1.000000000000000000 ) ) ;
#5279 = ORIENTED_EDGE ( 'NONE', *, *, #13687, .T. ) ;
#5280 = CARTESIAN_POINT ( 'NONE',  ( 2.000000000000004441, -21.29386353163882717, -12.16878555174548104 ) ) ;
#5281 = FACE_OUTER_BOUND ( 'NONE', #5438, .T. ) ;
#5282 = DIRECTION ( 'NONE',  ( -4.915049848600951133E-16, 0.000000000000000000, -1.000000000000000000 ) ) ;
#5283 = ORIENTED_EDGE ( 'NONE', *, *, #3163, .T. ) ;
#5284 = MECHANICAL_DESIGN_GEOMETRIC_PRESENTATION_REPRESENTATION (  '', ( #9417 ), #2050 ) ;
#5285 = CARTESIAN_POINT ( 'NONE',  ( 2.864755990943222308, 33.00319992234354771, -2.011557305968548093 ) ) ;
#5286 = CARTESIAN_POINT ( 'NONE',  ( -2.798362969681409851, 19.75319992234354416, -2.102939460078765421 ) ) ;
#5287 = AXIS2_PLACEMENT_3D ( 'NONE', #7405, #17078, #15581 ) ;
#5288 = VECTOR ( 'NONE', #4184, 1000.000000000000000 ) ;
#5289 = CARTESIAN_POINT ( 'NONE',  ( -2.121784821875005722, -23.22186879701663642, -2.475550400403212503 ) ) ;
#5290 = CARTESIAN_POINT ( 'NONE',  ( 2.518350579753628971, 31.87180007765648426, 0.7558219633769073242 ) ) ;
#5291 = CARTESIAN_POINT ( 'NONE',  ( 0.05938372350919016857, 25.12819992234354416, -4.731580009072201776 ) ) ;
#5292 = CARTESIAN_POINT ( 'NONE',  ( 1.999999999999994449, -27.76495267570075143, -9.331504893052493088 ) ) ;
#5293 = VERTEX_POINT ( 'NONE', #11158 ) ;
#5294 = EDGE_CURVE ( 'NONE', #15972, #1567, #5130, .T. ) ;
#5295 = CARTESIAN_POINT ( 'NONE',  ( 4.730628863548789710E-15, -15.82115571973984736, -6.856452161364834375 ) ) ;
#5296 = CARTESIAN_POINT ( 'NONE',  ( -3.673772985318219053, 35.74680007765646650, -2.599342558260952174 ) ) ;
#5297 = EDGE_CURVE ( 'NONE', #2086, #12341, #17608, .T. ) ;
#5298 = PRESENTATION_STYLE_ASSIGNMENT (( #15419 ) ) ;
#5299 = AXIS2_PLACEMENT_3D ( 'NONE', #10252, #14641, #1560 ) ;
#5300 = CARTESIAN_POINT ( 'NONE',  ( -4.243569643750004339, -26.62776571704792161, -9.475420353735756862 ) ) ;
#5301 = CARTESIAN_POINT ( 'NONE',  ( -4.000000000000000888, -26.04580080692037569, -12.91577843898463840 ) ) ;
#5302 = CARTESIAN_POINT ( 'NONE',  ( 4.000000000000003553, -19.42204459461930099, -7.482392114319592835 ) ) ;
#5303 = CARTESIAN_POINT ( 'NONE',  ( -1.999999999999996225, -20.47651710983858564, -11.00149388863366440 ) ) ;
#5304 = ORIENTED_EDGE ( 'NONE', *, *, #9531, .F. ) ;
#5305 = ORIENTED_EDGE ( 'NONE', *, *, #13683, .F. ) ;
#5306 = SHAPE_REPRESENTATION ( 'valve seat', ( #16940 ), #7446 ) ;
#5307 = CARTESIAN_POINT ( 'NONE',  ( -2.211161402132902243, 15.87180007765647716, -2.942372952327172886 ) ) ;
#5308 = CARTESIAN_POINT ( 'NONE',  ( -4.000000000000007105, 0.000000000000000000, -4.999999999999997335 ) ) ;
#5309 = CARTESIAN_POINT ( 'NONE',  ( 3.999999999999996447, -28.66886137708284110, -12.63557925674746762 ) ) ;
#5310 = CARTESIAN_POINT ( 'NONE',  ( 7.037197741572231990, -13.81849642415488688, -0.01350879608600348905 ) ) ;
#5311 = ORIENTED_EDGE ( 'NONE', *, *, #4354, .T. ) ;
#5312 = CARTESIAN_POINT ( 'NONE',  ( 0.8262555684460829442, 37.75319992234354771, -2.360188852285421302 ) ) ;
#5313 = AXIS2_PLACEMENT_3D ( 'NONE', #10981, #12184, #12454 ) ;
#5314 = CARTESIAN_POINT ( 'NONE',  ( 4.243569643749996345, -26.28361985523730837, -8.983929127162353367 ) ) ;
#5315 = CARTESIAN_POINT ( 'NONE',  ( 2.864755990943265829, 31.99680007765647716, 2.011557305968487697 ) ) ;
#5316 = AXIS2_PLACEMENT_3D ( 'NONE', #17534, #7479, #13227 ) ;
#5317 = CARTESIAN_POINT ( 'NONE',  ( -2.864755990943222308, 24.25319992234354416, 2.011557305968548093 ) ) ;
#5318 = FACE_OUTER_BOUND ( 'NONE', #17771, .T. ) ;
#5319 = CIRCLE ( 'NONE', #11217, 2.149999999999999023 ) ;
#5320 = CARTESIAN_POINT ( 'NONE',  ( -9.000000000000001776, 40.79999999999999716, 2.499999999999995559 ) ) ;
#5321 = CARTESIAN_POINT ( 'NONE',  ( 2.121784821874994176, -26.82464578784662379, -7.620849178593458007 ) ) ;
#5322 = EDGE_CURVE ( 'NONE', #9517, #6875, #13982, .T. ) ;
#5323 = DIRECTION ( 'NONE',  ( -3.373073425510457965E-16, 0.000000000000000000, -1.000000000000000000 ) ) ;
#5324 = CARTESIAN_POINT ( 'NONE',  ( -4.518350579753632523, 23.12180007765647005, -1.405661355842698468 ) ) ;
#5325 = VECTOR ( 'NONE', #12269, 1000.000000000000000 ) ;
#5326 = CARTESIAN_POINT ( 'NONE',  ( 9.000000000000005329, 16.59999999999999787, 2.499999999999997335 ) ) ;
#5327 = AXIS2_PLACEMENT_3D ( 'NONE', #2780, #5541, #11549 ) ;
#5328 = FACE_OUTER_BOUND ( 'NONE', #14739, .T. ) ;
#5329 = CARTESIAN_POINT ( 'NONE',  ( -4.243569643749997233, -20.33391164488314828, -9.029845429130588741 ) ) ;
#5330 = CARTESIAN_POINT ( 'NONE',  ( 3.999999999999996447, -26.60398620621909416, -9.686631897307085737 ) ) ;
#5331 = CARTESIAN_POINT ( 'NONE',  ( 0.000000000000000000, 43.00000000000000000, 2.500000000000000000 ) ) ;
#5332 = CARTESIAN_POINT ( 'NONE',  ( -1.989345975306426206, 37.74680007765647360, 1.515154207786343799 ) ) ;
#5333 = CARTESIAN_POINT ( 'NONE',  ( 1.533898589781675205E-14, -26.74131502120161841, -6.935288495286759058 ) ) ;
#5334 = CARTESIAN_POINT ( 'NONE',  ( -1.027846397803541700, 34.99680007765648071, 3.346150245485522312 ) ) ;
#5335 = CARTESIAN_POINT ( 'NONE',  ( -3.706921591972381904E-14, -16.89720386262061425, -6.824015130980216171 ) ) ;
#5336 = CARTESIAN_POINT ( 'NONE',  ( -3.313999109161785306, 15.00000000000000888, -2.150837222270006066 ) ) ;
#5337 = VERTEX_POINT ( 'NONE', #12558 ) ;
#5338 = CARTESIAN_POINT ( 'NONE',  ( -2.121784821874996396, -18.60988431229980833, -8.703424286353433459 ) ) ;
#5339 = CARTESIAN_POINT ( 'NONE',  ( 2.211161402132902243, 27.12180007765647360, 2.942372952327172442 ) ) ;
#5340 = DIRECTION ( 'NONE',  ( 0.000000000000000000, -1.000000000000000000, 9.859324684083080328E-16 ) ) ;
#5341 = CARTESIAN_POINT ( 'NONE',  ( 4.243569643750003451, -24.54969845206330703, -15.05061295465469762 ) ) ;
#5342 = DIRECTION ( 'NONE',  ( 1.000000000000000000, 0.000000000000000000, 0.000000000000000000 ) ) ;
#5343 = CARTESIAN_POINT ( 'NONE',  ( -8.000000000000001776, 25.39999999999999503, 2.499999999999995115 ) ) ;
#5344 = CARTESIAN_POINT ( 'NONE',  ( 9.000000000000000000, 27.59999999999999432, -2.500000000000001332 ) ) ;
#5345 = CARTESIAN_POINT ( 'NONE',  ( -4.243569643750005227, -27.91831269883777011, -11.31851245338599377 ) ) ;
#5346 = EDGE_CURVE ( 'NONE', #10567, #9202, #404, .T. ) ;
#5347 = EDGE_LOOP ( 'NONE', ( #2498, #14004, #148, #5582 ) ) ;
#5348 = CARTESIAN_POINT ( 'NONE',  ( 9.000000000000005329, -10.00000000000000000, 30.00000000000000000 ) ) ;
#5349 = CARTESIAN_POINT ( 'NONE',  ( -5.279047395330986450E-15, -24.92522350304378875, -3.262792381895696092 ) ) ;
#5350 = AXIS2_PLACEMENT_3D ( 'NONE', #13783, #11172, #18257 ) ;
#5351 = CARTESIAN_POINT ( 'NONE',  ( -2.798362969681365886, 37.74680007765647360, 2.102939460078824929 ) ) ;
#5352 = EDGE_CURVE ( 'NONE', #11426, #4161, #1619, .T. ) ;
#5353 = VERTEX_POINT ( 'NONE', #9775 ) ;
#5354 = CARTESIAN_POINT ( 'NONE',  ( -8.000000000000001776, 25.39999999999999503, 2.499999999999998224 ) ) ;
#5355 = APPLICATION_CONTEXT ( 'automotive_design' ) ;
#5356 = PRESENTATION_STYLE_ASSIGNMENT (( #3962 ) ) ;
#5357 = EDGE_CURVE ( 'NONE', #15102, #5921, #13432, .T. ) ;
#5358 = CARTESIAN_POINT ( 'NONE',  ( -4.481649420246396787, 37.12819992234354061, -1.518615910253363399 ) ) ;
#5359 = DIRECTION ( 'NONE',  ( -3.373073425510457965E-16, 0.000000000000000000, -1.000000000000000000 ) ) ;
#5360 = CARTESIAN_POINT ( 'NONE',  ( -0.8262555684460826111, 31.50319992234354416, 2.360188852285421302 ) ) ;
#5361 = ORIENTED_EDGE ( 'NONE', *, *, #16558, .T. ) ;
#5362 = CARTESIAN_POINT ( 'NONE',  ( 4.243569643750000786, -25.31986813001606862, -11.87903913343475892 ) ) ;
#5363 = ADVANCED_FACE ( 'NONE', ( #15619 ), #129, .T. ) ;
#5364 = CARTESIAN_POINT ( 'NONE',  ( 0.05938372350929014415, 22.37180007765647716, 4.731580009072201776 ) ) ;
#5365 = CARTESIAN_POINT ( 'NONE',  ( -1.999999999999996225, -17.83089579646446410, -7.223155083343911542 ) ) ;
#5366 = EDGE_LOOP ( 'NONE', ( #15916, #14016, #5448, #14530 ) ) ;
#5367 = VECTOR ( 'NONE', #12183, 1000.000000000000000 ) ;
#5368 = DIRECTION ( 'NONE',  ( -0.000000000000000000, 0.000000000000000000, -1.000000000000000000 ) ) ;
#5369 = EDGE_CURVE ( 'NONE', #17169, #7294, #16191, .T. ) ;
#5370 = DIRECTION ( 'NONE',  ( 0.000000000000000000, 0.000000000000000000, -1.000000000000000000 ) ) ;
#5371 = CARTESIAN_POINT ( 'NONE',  ( -11.99999999999999822, 48.00000000000000000, 15.00000000000000000 ) ) ;
#5372 = CARTESIAN_POINT ( 'NONE',  ( -5.330712181944245322E-15, -27.33340804591119522, -6.211691927533303570 ) ) ;
#5373 = CARTESIAN_POINT ( 'NONE',  ( 4.898587196589413815E-16, 2.700915433685006750, 35.11257424290206330 ) ) ;
#5374 = VERTEX_POINT ( 'NONE', #8553 ) ;
#5375 = CARTESIAN_POINT ( 'NONE',  ( 2.000000000000004441, -21.03575413528086102, -11.80016713181543331 ) ) ;
#5376 = CARTESIAN_POINT ( 'NONE',  ( 3.999999999999996447, -27.05567764914059481, -10.33171413117790394 ) ) ;
#5377 = CARTESIAN_POINT ( 'NONE',  ( -2.864755990943265829, 15.74680007765647716, -2.011557305968488141 ) ) ;
#5378 = ORIENTED_EDGE ( 'NONE', *, *, #8416, .T. ) ;
#5379 =( GEOMETRIC_REPRESENTATION_CONTEXT ( 3 ) GLOBAL_UNCERTAINTY_ASSIGNED_CONTEXT ( ( #8113 ) ) GLOBAL_UNIT_ASSIGNED_CONTEXT ( ( #13700, #742, #6385 ) ) REPRESENTATION_CONTEXT ( 'NONE', 'WORKASPACE' ) );
#5380 = CARTESIAN_POINT ( 'NONE',  ( 3.481649420246394122, 33.37819992234353350, 1.193696214020467439 ) ) ;
#5381 = CARTESIAN_POINT ( 'NONE',  ( 2.115076519116425580, 16.12819992234354416, 3.012182706137062294 ) ) ;
#5382 = CARTESIAN_POINT ( 'NONE',  ( 4.243569643750000786, -20.38352592466991808, -4.829211852272596417 ) ) ;
#5383 = CARTESIAN_POINT ( 'NONE',  ( -0.8262555684461330152, 33.49680007765648071, -2.360188852285403982 ) ) ;
#5384 = CARTESIAN_POINT ( 'NONE',  ( -2.829195390882724315, 26.62819992234354416, 3.793023760679264722 ) ) ;
#5385 = CARTESIAN_POINT ( 'NONE',  ( -3.999999999999997335, -22.36879353566782669, -11.69078574084754152 ) ) ;
#5386 = VERTEX_POINT ( 'NONE', #323 ) ;
#5387 = VECTOR ( 'NONE', #15492, 1000.000000000000000 ) ;
#5388 = CARTESIAN_POINT ( 'NONE',  ( -2.121784821874996396, -17.31933733050996338, -6.860332186703194779 ) ) ;
#5389 = CARTESIAN_POINT ( 'NONE',  ( -1.135272562821090014, 23.49680007765647716, -3.311245368580554072 ) ) ;
#5390 = SURFACE_SIDE_STYLE ('',( #4083 ) ) ;
#5391 = PRESENTATION_LAYER_ASSIGNMENT (  '', '', ( #2153 ) ) ;
#5392 = CARTESIAN_POINT ( 'NONE',  ( -2.121784821874996396, -20.38438641226084158, -11.23767592337251209 ) ) ;
#5393 = CARTESIAN_POINT ( 'NONE',  ( 4.000000000000000888, -24.36808973059358863, -10.51975870943932456 ) ) ;
#5394 = CARTESIAN_POINT ( 'NONE',  ( -3.999999999999997335, -21.40088330003039019, -10.30846666711662962 ) ) ;
#5395 = ORIENTED_EDGE ( 'NONE', *, *, #13177, .T. ) ;
#5396 = ORIENTED_EDGE ( 'NONE', *, *, #8693, .F. ) ;
#5397 = CARTESIAN_POINT ( 'NONE',  ( 3.518350579753631191, 16.87180007765648071, 1.080741659609802285 ) ) ;
#5398 = CARTESIAN_POINT ( 'NONE',  ( 3.579096709490575479E-14, -25.12813129325936501, -4.631423369717193594 ) ) ;
#5399 = CIRCLE ( 'NONE', #676, 0.9999999999999991118 ) ;
#5400 = CARTESIAN_POINT ( 'NONE',  ( 1.300000000000000044, 1.877893248421448789E-16, 1.250000000000000000 ) ) ;
#5401 = CARTESIAN_POINT ( 'NONE',  ( -1.071796769724494114, -30.10826387457404607, -11.74378978903329518 ) ) ;
#5402 = ORIENTED_EDGE ( 'NONE', *, *, #1921, .T. ) ;
#5403 = COLOUR_RGB ( '',1.000000000000000000, 0.9490196078431372140, 0.9098039215686274384 ) ;
#5404 = CARTESIAN_POINT ( 'NONE',  ( -1.593127413382952939, 39.12819992234354771, 2.091722143975172532 ) ) ;
#5405 = CARTESIAN_POINT ( 'NONE',  ( -2.121784821875005722, -26.83540034602819802, -7.636208279423879475 ) ) ;
#5406 = CARTESIAN_POINT ( 'NONE',  ( -2.211161402132902243, 33.37180007765648071, -2.942372952327172886 ) ) ;
#5407 =( GEOMETRIC_REPRESENTATION_CONTEXT ( 3 ) GLOBAL_UNCERTAINTY_ASSIGNED_CONTEXT ( ( #2509 ) ) GLOBAL_UNIT_ASSIGNED_CONTEXT ( ( #16475, #4964, #992 ) ) REPRESENTATION_CONTEXT ( 'NONE', 'WORKASPACE' ) );
#5408 = CARTESIAN_POINT ( 'NONE',  ( 1.027846397803612311, 26.25319992234354771, 3.346150245485499219 ) ) ;
#5409 = CARTESIAN_POINT ( 'NONE',  ( 9.000000000000005329, -10.00000000000000000, -3.713574246709344884 ) ) ;
#5410 = CARTESIAN_POINT ( 'NONE',  ( -1.734723475976807094E-15, 34.19999999999999574, -2.500000000000000000 ) ) ;
#5411=STYLED_ITEM('',(#18396),#8199);
#5412 = CARTESIAN_POINT ( 'NONE',  ( -2.121784821874996396, -21.70719706859543408, -13.12684532551400629 ) ) ;
#5413 = AXIS2_PLACEMENT_3D ( 'NONE', #396, #1351, #4641 ) ;
#5414 =( BOUNDED_CURVE ( )  B_SPLINE_CURVE ( 2, ( #17535, #17437, #5997, #4702, #11651, #8771, #7758, #4799, #10450 ),
 .UNSPECIFIED., .F., .F. ) 
 B_SPLINE_CURVE_WITH_KNOTS ( ( 3, 2, 2, 2, 3 ),
 ( 0.4396551724137931494, 0.4425287356321839227, 0.4482758620689655249, 0.4540229885057471271, 0.4568965517241379559 ),
 .UNSPECIFIED. ) 
 CURVE ( )  GEOMETRIC_REPRESENTATION_ITEM ( )  RATIONAL_B_SPLINE_CURVE ( ( 0.9330127018922194093, 0.9330127018922200755, 1.000000000000000000, 0.8660254037844387076, 1.000000000000000000, 0.8660254037844387076, 1.000000000000000000, 0.9330127018922187432, 0.9330127018922194093 ) ) 
 REPRESENTATION_ITEM ( '' )  );
#5415 = CARTESIAN_POINT ( 'NONE',  ( -6.938893903907228378E-15, 6.938893903907228378E-15, -30.00000000000000000 ) ) ;
#5416 = ADVANCED_FACE ( 'NONE', ( #43 ), #6346, .F. ) ;
#5417 = DIRECTION ( 'NONE',  ( 0.000000000000000000, 0.000000000000000000, -1.000000000000000000 ) ) ;
#5418 = CARTESIAN_POINT ( 'NONE',  ( 4.730628863548789710E-15, -18.62809540513275408, -10.86517747810410306 ) ) ;
#5419 = DIRECTION ( 'NONE',  ( 0.000000000000000000, 0.000000000000000000, 1.000000000000000000 ) ) ;
#5420 =( LENGTH_UNIT ( ) NAMED_UNIT ( * ) SI_UNIT ( .MILLI., .METRE. ) );
#5421 = CARTESIAN_POINT ( 'NONE',  ( 2.055738996568313048, 36.99680007765647360, 1.423772053676023441 ) ) ;
#5422 = EDGE_CURVE ( 'NONE', #2131, #9627, #5434, .T. ) ;
#5423 = DIRECTION ( 'NONE',  ( 0.000000000000000000, 0.000000000000000000, -1.000000000000000000 ) ) ;
#5424 = CARTESIAN_POINT ( 'NONE',  ( 2.798362969681366330, 33.99680007765648071, -2.102939460078824929 ) ) ;
#5425 = CARTESIAN_POINT ( 'NONE',  ( -1.999999999999996225, -22.47686493090789739, -13.85828664208477079 ) ) ;
#5426 = AXIS2_PLACEMENT_3D ( 'NONE', #7002, #153, #15922 ) ;
#5427 = CIRCLE ( 'NONE', #10746, 4.000000000000001776 ) ;
#5428 = DIRECTION ( 'NONE',  ( 3.469446951953612217E-16, -0.000000000000000000, 1.000000000000000000 ) ) ;
#5429 = VERTEX_POINT ( 'NONE', #14409 ) ;
#5430 = CARTESIAN_POINT ( 'NONE',  ( -2.121784821875005722, -23.77035126427731981, -3.258864542754563942 ) ) ;
#5431 = CARTESIAN_POINT ( 'NONE',  ( -2.864755990943265829, 20.74680007765647716, -2.011557305968488141 ) ) ;
#5432 = CARTESIAN_POINT ( 'NONE',  ( -2.694913683823399353, -10.54254386713301805, 22.30101802474215233 ) ) ;
#5433 = DIRECTION ( 'NONE',  ( -0.000000000000000000, 1.000000000000000000, -0.000000000000000000 ) ) ;
#5434 = CIRCLE ( 'NONE', #11960, 10.00000000000000000 ) ;
#5435 = DIRECTION ( 'NONE',  ( -1.000000000000000000, -0.000000000000000000, -0.000000000000000000 ) ) ;
#5436 = DIRECTION ( 'NONE',  ( -1.000000000000000000, -0.000000000000000000, -0.000000000000000000 ) ) ;
#5437 = CARTESIAN_POINT ( 'NONE',  ( 4.243569643750003451, -23.77537026298940148, -13.94475769486455619 ) ) ;
#5438 = EDGE_LOOP ( 'NONE', ( #1952, #5150, #11804, #1996 ) ) ;
#5439 = CARTESIAN_POINT ( 'NONE',  ( -1.071796769724496334, -20.24109931455537392, -11.59959275541492119 ) ) ;
#5440 = CARTESIAN_POINT ( 'NONE',  ( -5.279047395330986450E-15, -25.44144229575972460, -4.000029221755790232 ) ) ;
#5441 = CARTESIAN_POINT ( 'NONE',  ( 1.989345975306426206, 16.49680007765648071, -1.515154207786343799 ) ) ;
#5442 = ORIENTED_EDGE ( 'NONE', *, *, #1984, .T. ) ;
#5443 = CARTESIAN_POINT ( 'NONE',  ( -5.577813053751546416E-15, -23.90211166126395881, -2.880485876056233518 ) ) ;
#5444 =( NAMED_UNIT ( * ) SI_UNIT ( $, .STERADIAN. ) SOLID_ANGLE_UNIT ( ) );
#5445 = CARTESIAN_POINT ( 'NONE',  ( -4.518350579753632523, 18.12180007765647716, -1.405661355842698468 ) ) ;
#5446 = DIRECTION ( 'NONE',  ( -1.000000000000000000, 0.000000000000000000, 0.000000000000000000 ) ) ;
#5447 = CARTESIAN_POINT ( 'NONE',  ( 1.593127413382953383, 27.87819992234355126, -2.091722143975172532 ) ) ;
#5448 = ORIENTED_EDGE ( 'NONE', *, *, #16149, .F. ) ;
#5449 = CARTESIAN_POINT ( 'NONE',  ( -2.121784821875005722, -29.19064858779466221, -10.99985136128556462 ) ) ;
#5450 = CARTESIAN_POINT ( 'NONE',  ( 4.481649420246366589, 26.62180007765648426, -1.518615910253458212 ) ) ;
#5451 = CARTESIAN_POINT ( 'NONE',  ( -4.000000000000000888, -21.39983167247694240, -6.280646880243780039 ) ) ;
#5452 = CIRCLE ( 'NONE', #13736, 2.000000000000001776 ) ;
#5453 = ORIENTED_EDGE ( 'NONE', *, *, #17696, .F. ) ;
#5454 = ADVANCED_FACE ( 'NONE', ( #17030, #14131 ), #1444, .T. ) ;
#5455 = DIRECTION ( 'NONE',  ( -0.000000000000000000, -1.000000000000000000, -0.000000000000000000 ) ) ;
#5456 = CARTESIAN_POINT ( 'NONE',  ( -1.999999999999996225, -21.25084529891249119, -12.10734914842380761 ) ) ;
#5457 = DIRECTION ( 'NONE',  ( -0.000000000000000000, -0.5735764363510414965, -0.8191520442889950182 ) ) ;
#5458 = FACE_OUTER_BOUND ( 'NONE', #14187, .T. ) ;
#5459 = CARTESIAN_POINT ( 'NONE',  ( -4.243569643749997233, -20.88239411214383523, -9.813159571481939736 ) ) ;
#5460 = EDGE_LOOP ( 'NONE', ( #17529, #8611, #14442, #8441 ) ) ;
#5461 = CARTESIAN_POINT ( 'NONE',  ( -8.500000000000005329, 10.00000000000000000, -20.49999999999999645 ) ) ;
#5462 = VERTEX_POINT ( 'NONE', #11337 ) ;
#5463 = CARTESIAN_POINT ( 'NONE',  ( -5.279047395330986450E-15, -28.53875505205535035, -8.423450260916363064 ) ) ;
#5464 = CYLINDRICAL_SURFACE ( 'NONE', #3017, 4.000000000000000000 ) ;
#5465 = CARTESIAN_POINT ( 'NONE',  ( 3.481649420246370141, 16.62180007765647716, -1.193696214020541602 ) ) ;
#5466 =( NAMED_UNIT ( * ) PLANE_ANGLE_UNIT ( ) SI_UNIT ( $, .RADIAN. ) );
#5467 = ORIENTED_EDGE ( 'NONE', *, *, #16182, .F. ) ;
#5468 = CARTESIAN_POINT ( 'NONE',  ( 1.027846397803612311, 33.75319992234354771, 3.346150245485499219 ) ) ;
#5469 = CARTESIAN_POINT ( 'NONE',  ( -2.864755990943222308, 16.75319992234354416, 2.011557305968548093 ) ) ;
#5470 = CARTESIAN_POINT ( 'NONE',  ( 4.000000000000003553, -24.32612312542070754, -14.48614209299049804 ) ) ;
#5471 = CARTESIAN_POINT ( 'NONE',  ( -1.593127413382998459, 28.37180007765648426, -2.091722143975139669 ) ) ;
#5472 = CARTESIAN_POINT ( 'NONE',  ( 1.336863392178569754, 28.75319992234354771, 4.297206761780648421 ) ) ;
#5473 = UNCERTAINTY_MEASURE_WITH_UNIT (LENGTH_MEASURE( 1.000000000000000082E-05 ), #13339, 'distance_accuracy_value', 'NONE');
#5474 = CARTESIAN_POINT ( 'NONE',  ( -5.279047395330986450E-15, -28.73233709861888485, -8.699914074857131752 ) ) ;
#5475 = VERTEX_POINT ( 'NONE', #15710 ) ;
#5476 = ADVANCED_FACE ( 'NONE', ( #4300 ), #17904, .T. ) ;
#5477 = ADVANCED_FACE ( 'NONE', ( #1532 ), #7506, .T. ) ;
#5478 = CARTESIAN_POINT ( 'NONE',  ( 3.250767888004682415, -21.90484815091188509, -2.246271217071878823 ) ) ;
#5479 = EDGE_CURVE ( 'NONE', #4093, #7588, #4392, .T. ) ;
#5480 = CARTESIAN_POINT ( 'NONE',  ( -3.481649420246369697, 22.87180007765647360, 1.193696214020542490 ) ) ;
#5481 = DIRECTION ( 'NONE',  ( 1.000000000000000000, 0.000000000000000000, 0.000000000000000000 ) ) ;
#5482 = CARTESIAN_POINT ( 'NONE',  ( 2.121784821874994176, -26.27616332058593684, -6.837535036242106123 ) ) ;
#5483 = CARTESIAN_POINT ( 'NONE',  ( 4.000000000000003553, -22.45483000112048799, -11.81365854749088840 ) ) ;
#5484 = CARTESIAN_POINT ( 'NONE',  ( 1.071796769724476128, -17.68305875241334491, -7.946332225426282037 ) ) ;
#5485 = CARTESIAN_POINT ( 'NONE',  ( -1.734723475976807094E-15, 25.39999999999999503, -10.50000000000000178 ) ) ;
#5486 = ORIENTED_EDGE ( 'NONE', *, *, #12314, .F. ) ;
#5487 = ORIENTED_EDGE ( 'NONE', *, *, #9824, .F. ) ;
#5488 = CARTESIAN_POINT ( 'NONE',  ( 9.000000000000001776, 31.99999999999999289, -2.500000000000002665 ) ) ;
#5489 = CARTESIAN_POINT ( 'NONE',  ( 8.000000000000000000, 38.59999999999999432, -2.500000000000000888 ) ) ;
#5490 = DIRECTION ( 'NONE',  ( 0.000000000000000000, 0.000000000000000000, 1.000000000000000000 ) ) ;
#5491 = CARTESIAN_POINT ( 'NONE',  ( -1.734723475976807094E-15, 18.79999999999999361, -2.500000000000000000 ) ) ;
#5492 = ORIENTED_EDGE ( 'NONE', *, *, #13638, .T. ) ;
#5493 = CARTESIAN_POINT ( 'NONE',  ( -0.8262555684460826111, 39.00319992234355482, 2.360188852285421302 ) ) ;
#5494 = CARTESIAN_POINT ( 'NONE',  ( -5.330712181944245322E-15, -28.59169135315628907, -8.008706724692286727 ) ) ;
#5495 = CARTESIAN_POINT ( 'NONE',  ( 3.481649420246369697, 29.12180007765647005, -1.193696214020541824 ) ) ;
#5496 = CARTESIAN_POINT ( 'NONE',  ( 3.500000000000000444, 25.75319992234354771, 0.05647727720529520379 ) ) ;
#5497 = CARTESIAN_POINT ( 'NONE',  ( 9.999999999999998224, 43.00000000000000000, -2.500000000000001776 ) ) ;
#5498 = FACE_OUTER_BOUND ( 'NONE', #6297, .T. ) ;
#5499 = CARTESIAN_POINT ( 'NONE',  ( 2.121784821875004390, -20.45966831953192511, -11.34518962918543927 ) ) ;
#5500 = LINE ( 'NONE', #2823, #14123 ) ;
#5501 = ADVANCED_FACE ( 'NONE', ( #12912 ), #7803, .T. ) ;
#5502 = CARTESIAN_POINT ( 'NONE',  ( 0.000000000000000000, 5.000000000000000000, -4.000000000000001776 ) ) ;
#5503 = CARTESIAN_POINT ( 'NONE',  ( 2.399999999999999911, 0.000000000000000000, 2.200000000000000178 ) ) ;
#5504 = CARTESIAN_POINT ( 'NONE',  ( -4.243569643750005227, -24.30478114982620497, -6.157854574365327238 ) ) ;
#5505 = AXIS2_PLACEMENT_3D ( 'NONE', #12353, #16555, #8184 ) ;
#5506 = CARTESIAN_POINT ( 'NONE',  ( 3.999999999999993339, 7.428752623566170548E-15, 30.00000000000000000 ) ) ;
#5507 = CARTESIAN_POINT ( 'NONE',  ( 2.481649420246391902, 15.87819992234354771, 0.8687765177875720335 ) ) ;
#5508 = TOROIDAL_SURFACE ( 'NONE', #4631, 9.000000000000001776, 0.9999999999999991118 ) ;
#5509 = CARTESIAN_POINT ( 'NONE',  ( -1.999999999999996225, -19.37955217461227875, -9.434865602924197958 ) ) ;
#5510 = CARTESIAN_POINT ( 'NONE',  ( -3.481649420246370141, 35.37180007765648071, 1.193696214020542268 ) ) ;
#5511 = CARTESIAN_POINT ( 'NONE',  ( 1.071796769724485232, -29.05277288770450639, -10.23639244000127135 ) ) ;
#5512 = ITEM_DEFINED_TRANSFORMATION ( 'NONE', 'NONE', #14892,  #16940 ) ;
#5513 = DIRECTION ( 'NONE',  ( -1.000000000000000000, -0.000000000000000000, -0.000000000000000000 ) ) ;
#5514 = ORIENTED_EDGE ( 'NONE', *, *, #16181, .T. ) ;
#5515 = CARTESIAN_POINT ( 'NONE',  ( 2.121784821875004390, -18.13668375231020846, -8.027623849815011425 ) ) ;
#5516 = CARTESIAN_POINT ( 'NONE',  ( 3.481649420246369697, 29.12180007765647005, -1.193696214020541824 ) ) ;
#5517 =( BOUNDED_CURVE ( )  B_SPLINE_CURVE ( 2, ( #8588, #7201, #1046, #11370, #7111, #9561, #17060, #15240, #6685 ),
 .UNSPECIFIED., .F., .T. ) 
 B_SPLINE_CURVE_WITH_KNOTS ( ( 3, 2, 2, 2, 3 ),
 ( 0.1293103448275862155, 0.1321839080459770166, 0.1379310344827586188, 0.1436781609195402210, 0.1465517241379310498 ),
 .UNSPECIFIED. ) 
 CURVE ( )  GEOMETRIC_REPRESENTATION_ITEM ( )  RATIONAL_B_SPLINE_CURVE ( ( 0.9330127018922194093, 0.9330127018922194093, 1.000000000000000000, 0.8660254037844387076, 1.000000000000000000, 0.8660254037844387076, 1.000000000000000000, 0.9330127018922189652, 0.9330127018922192983 ) ) 
 REPRESENTATION_ITEM ( '' )  );
#5518 = EDGE_CURVE ( 'NONE', #7315, #4695, #17212, .T. ) ;
#5519 = FACE_OUTER_BOUND ( 'NONE', #16171, .T. ) ;
#5520 = EDGE_CURVE ( 'NONE', #12007, #11229, #16724, .T. ) ;
#5521 = CARTESIAN_POINT ( 'NONE',  ( -4.243569643749998122, -24.72177138296861898, -15.29635856794140025 ) ) ;
#5522 = CARTESIAN_POINT ( 'NONE',  ( 9.999999999999998224, 38.59999999999999432, -2.500000000000001776 ) ) ;
#5523 = CARTESIAN_POINT ( 'NONE',  ( -1.734723475976807094E-15, 23.19999999999999574, -10.50000000000000178 ) ) ;
#5524 = CARTESIAN_POINT ( 'NONE',  ( -8.500000000000005329, 15.00000000000000178, -18.35000000000000142 ) ) ;
#5525 = CARTESIAN_POINT ( 'NONE',  ( -2.121784821874996396, -23.73980856491443703, -16.02971538246313443 ) ) ;
#5526 = EDGE_LOOP ( 'NONE', ( #13577, #4759 ) ) ;
#5527 = CARTESIAN_POINT ( 'NONE',  ( 9.000000000000000000, 16.59999999999999787, -2.500000000000001332 ) ) ;
#5528 = CARTESIAN_POINT ( 'NONE',  ( -5.279047395330986450E-15, -25.18333289940175845, -3.631410801825742496 ) ) ;
#5529 = CARTESIAN_POINT ( 'NONE',  ( 1.497042530366477164, 16.37180007765648426, -2.161531897785062384 ) ) ;
#5530 = ORIENTED_EDGE ( 'NONE', *, *, #4168, .T. ) ;
#5531 = CARTESIAN_POINT ( 'NONE',  ( 2.000000000000004441, -22.58441051342866857, -14.01187765139572150 ) ) ;
#5532 = CARTESIAN_POINT ( 'NONE',  ( 4.518350579753633411, 16.87180007765647716, 1.405661355842698468 ) ) ;
#5533 = CARTESIAN_POINT ( 'NONE',  ( 4.000000000000000000, 0.000000000000000000, 0.000000000000000000 ) ) ;
#5534 = CIRCLE ( 'NONE', #6709, 0.9999999999999991118 ) ;
#5535 = CARTESIAN_POINT ( 'NONE',  ( -2.500000000000001332, 39.50319992234355482, -0.05647727720530596601 ) ) ;
#5536 = ORIENTED_EDGE ( 'NONE', *, *, #10577, .F. ) ;
#5537 = CARTESIAN_POINT ( 'NONE',  ( -2.121784821874996396, -21.96530646495340378, -13.49546374544405403 ) ) ;
#5538 = CARTESIAN_POINT ( 'NONE',  ( -0.05938372350928957516, 26.12180007765648426, -4.731580009072201776 ) ) ;
#5539 = EDGE_CURVE ( 'NONE', #5080, #15989, #4665, .T. ) ;
#5540 = ORIENTED_EDGE ( 'NONE', *, *, #14255, .T. ) ;
#5541 = DIRECTION ( 'NONE',  ( 1.000000000000000000, -0.000000000000000000, 0.000000000000000000 ) ) ;
#5542 = EDGE_CURVE ( 'NONE', #10845, #13534, #7210, .T. ) ;
#5543 = CARTESIAN_POINT ( 'NONE',  ( -1.734723475976807094E-15, 29.79999999999999716, -2.500000000000000000 ) ) ;
#5544 = TOROIDAL_SURFACE ( 'NONE', #10878, 9.000000000000003553, 0.9999999999999991118 ) ;
#5545 = DIRECTION ( 'NONE',  ( -0.000000000000000000, 1.000000000000000000, -0.000000000000000000 ) ) ;
#5546 = CIRCLE ( 'NONE', #15923, 3.047499999999999876 ) ;
#5547 =( BOUNDED_CURVE ( )  B_SPLINE_CURVE ( 2, ( #11868, #8804, #17561, #14768, #14863, #2067, #9454, #6494, #10843 ),
 .UNSPECIFIED., .F., .F. ) 
 B_SPLINE_CURVE_WITH_KNOTS ( ( 3, 2, 2, 2, 3 ),
 ( 0.6465517241379310498, 0.6494252873563218786, 0.6551724137931034253, 0.6609195402298850830, 0.6637931034482759118 ),
 .UNSPECIFIED. ) 
 CURVE ( )  GEOMETRIC_REPRESENTATION_ITEM ( )  RATIONAL_B_SPLINE_CURVE ( ( 0.9330127018922194093, 0.9330127018922194093, 1.000000000000000000, 0.8660254037844387076, 1.000000000000000000, 0.8660254037844387076, 1.000000000000000000, 0.9330127018922180770, 0.9330127018922194093 ) ) 
 REPRESENTATION_ITEM ( '' )  );
#5548 = CARTESIAN_POINT ( 'NONE',  ( 4.243569643749996345, -24.25100835891830542, -6.081059070213228779 ) ) ;
#5549 = ORIENTED_EDGE ( 'NONE', *, *, #3031, .F. ) ;
#5550 = CARTESIAN_POINT ( 'NONE',  ( 15.00000000000000355, -4.000000000000000000, 30.00000000000000000 ) ) ;
#5551 = ORIENTED_EDGE ( 'NONE', *, *, #210, .F. ) ;
#5552 = CARTESIAN_POINT ( 'NONE',  ( -4.000000000000004441, -26.69002267167174125, -9.809504703950437943 ) ) ;
#5553 = CARTESIAN_POINT ( 'NONE',  ( 9.999999999999998224, 29.79999999999999716, -2.500000000000001776 ) ) ;
#5554 = DIRECTION ( 'NONE',  ( 0.000000000000000000, 0.000000000000000000, 1.000000000000000000 ) ) ;
#5555 = SURFACE_STYLE_FILL_AREA ( #4341 ) ;
#5556 = CARTESIAN_POINT ( 'NONE',  ( -2.733110507866328476, 14.87819992234354238, -3.862833514489096398 ) ) ;
#5557 = CARTESIAN_POINT ( 'NONE',  ( -3.500000000000000444, 17.00319992234354416, -0.05647727720529563400 ) ) ;
#5558 = CARTESIAN_POINT ( 'NONE',  ( 1.999999999999994449, -29.12002700728503513, -11.26675159869200904 ) ) ;
#5559 = CARTESIAN_POINT ( 'NONE',  ( -1.989345975306426206, 35.24680007765648071, 1.515154207786343799 ) ) ;
#5560 = CIRCLE ( 'NONE', #9391, 0.9999999999999991118 ) ;
#5561 = CARTESIAN_POINT ( 'NONE',  ( -1.444289557195956863, 26.50319992234354771, 4.262301884875733471 ) ) ;
#5562 = VECTOR ( 'NONE', #4380, 1000.000000000000000 ) ;
#5563 = CARTESIAN_POINT ( 'NONE',  ( -5.279047395330986450E-15, -27.95800890954496865, -7.594058815066988544 ) ) ;
#5564 = ORIENTED_EDGE ( 'NONE', *, *, #16531, .T. ) ;
#5565 = CARTESIAN_POINT ( 'NONE',  ( -1.071796769724486786, -22.37050183521355962, -14.64069472084458035 ) ) ;
#5566 = CARTESIAN_POINT ( 'NONE',  ( 2.798362969681366330, 21.49680007765647716, -2.102939460078824929 ) ) ;
#5567 = CARTESIAN_POINT ( 'NONE',  ( 4.243569643750003451, -21.45238569576768484, -10.62719191549412656 ) ) ;
#5568 = CIRCLE ( 'NONE', #14160, 0.9999999999999991118 ) ;
#5569 = CARTESIAN_POINT ( 'NONE',  ( -1.999999999999996225, -22.02517348798640029, -13.21320440821394904 ) ) ;
#5570 = MECHANICAL_DESIGN_GEOMETRIC_PRESENTATION_REPRESENTATION (  '', ( #14771 ), #3504 ) ;
#5571 = CARTESIAN_POINT ( 'NONE',  ( 1.533898589781675205E-14, -26.74131502120161841, -6.935288495286759058 ) ) ;
#5572 = VERTEX_POINT ( 'NONE', #14513 ) ;
#5573 = AXIS2_PLACEMENT_3D ( 'NONE', #121, #9853, #2825 ) ;
#5574 = ORIENTED_EDGE ( 'NONE', *, *, #13117, .T. ) ;
#5575 = CARTESIAN_POINT ( 'NONE',  ( 2.798362969681366330, 26.49680007765648071, -2.102939460078824929 ) ) ;
#5576 = B_SPLINE_CURVE_WITH_KNOTS ( 'NONE', 1,
 ( #13305, #4867 ),
 .UNSPECIFIED., .F., .F.,
 ( 2, 2 ),
 ( 0.000000000000000000, 0.9777443369282337038 ),
 .UNSPECIFIED. ) ;
#5577 = DIRECTION ( 'NONE',  ( 0.000000000000000000, 0.000000000000000000, 1.000000000000000000 ) ) ;
#5578 = ADVANCED_FACE ( 'NONE', ( #1912 ), #14705, .F. ) ;
#5579 = SURFACE_STYLE_USAGE ( .BOTH. , #4459 ) ;
#5580 = CARTESIAN_POINT ( 'NONE',  ( 8.499999999999994671, 14.99364916731036956, 18.35000000000000142 ) ) ;
#5581 = CARTESIAN_POINT ( 'NONE',  ( 1.999999999999994449, -25.76460485463143968, -6.474712139601389360 ) ) ;
#5582 = ORIENTED_EDGE ( 'NONE', *, *, #11127, .F. ) ;
#5583 = CARTESIAN_POINT ( 'NONE',  ( 2.864755990943222308, 15.50319992234354416, -2.011557305968548093 ) ) ;
#5584 = ADVANCED_FACE ( 'NONE', ( #13194, #9119 ), #11897, .F. ) ;
#5585 = CARTESIAN_POINT ( 'NONE',  ( 4.730628863548789710E-15, -19.40242359420666318, -11.97103273789424449 ) ) ;
#5586 = CARTESIAN_POINT ( 'NONE',  ( 3.518350579753631191, 34.37180007765648071, 1.080741659609802285 ) ) ;
#5587 = EDGE_CURVE ( 'NONE', #94, #12048, #8835, .T. ) ;
#5588 = CARTESIAN_POINT ( 'NONE',  ( 2.864755990943222308, 25.50319992234354771, -2.011557305968548093 ) ) ;
#5589 = DIRECTION ( 'NONE',  ( 0.000000000000000000, 0.000000000000000000, -1.000000000000000000 ) ) ;
#5590 = DIRECTION ( 'NONE',  ( -1.000000000000000000, 0.000000000000000000, -0.000000000000000000 ) ) ;
#5591 = EDGE_CURVE ( 'NONE', #2571, #8991, #9215, .T. ) ;
#5592=STYLED_ITEM('',(#18396),#14621);
#5593 = CARTESIAN_POINT ( 'NONE',  ( 4.243569643750000786, -24.02932114822622722, -10.03594703378452024 ) ) ;
#5594 = VECTOR ( 'NONE', #16059, 999.9999999999998863 ) ;
#5595 = EDGE_CURVE ( 'NONE', #5047, #4253, #1810, .T. ) ;
#5596 = CARTESIAN_POINT ( 'NONE',  ( 0.000000000000000000, -9.999999999999998224, -3.075850967158335614 ) ) ;
#5597 = CARTESIAN_POINT ( 'NONE',  ( 8.000000000000000000, 46.00000000000000000, 2.500000000000000000 ) ) ;
#5598 = CARTESIAN_POINT ( 'NONE',  ( -4.243569643749997233, -18.26903647401939779, -6.080898069690205965 ) ) ;
#5599 = PRODUCT_DEFINITION ( 'UNKNOWN', '', #9538, #12661 ) ;
#5600 = DIRECTION ( 'NONE',  ( -0.000000000000000000, -0.5735764363510414965, -0.8191520442889950182 ) ) ;
#5601 = DIRECTION ( 'NONE',  ( -0.000000000000000000, 1.000000000000000000, -0.000000000000000000 ) ) ;
#5602 = ORIENTED_EDGE ( 'NONE', *, *, #17851, .F. ) ;
#5603 = AXIS2_PLACEMENT_3D ( 'NONE', #13135, #4601, #3319 ) ;
#5604 = CARTESIAN_POINT ( 'NONE',  ( 0.05938372350926800214, 34.87180007765648071, 2.628655560595669183 ) ) ;
#5605 = CARTESIAN_POINT ( 'NONE',  ( -2.000000000000005773, -24.96876754848942070, -5.338138677143647648 ) ) ;
#5606 = CARTESIAN_POINT ( 'NONE',  ( -3.500000000000000444, 40.49680007765648071, 0.05647727720536853402 ) ) ;
#5607 = ITEM_DEFINED_TRANSFORMATION ( 'NONE', 'NONE', #8349,  #16940 ) ;
#5608 = EDGE_LOOP ( 'NONE', ( #13833, #16361, #11582, #2797 ) ) ;
#5609 = CARTESIAN_POINT ( 'NONE',  ( -2.121784821874996396, -16.80311853779403108, -6.123095346843099307 ) ) ;
#5610 = CARTESIAN_POINT ( 'NONE',  ( -3.481649420246369697, 30.37180007765647005, 1.193696214020542490 ) ) ;
#5611 = AXIS2_PLACEMENT_3D ( 'NONE', #3576, #7738, #9226 ) ;
#5612 = AXIS2_PLACEMENT_3D ( 'NONE', #15653, #448, #10352 ) ;
#5613 = DIRECTION ( 'NONE',  ( 0.000000000000000000, 0.000000000000000000, 1.000000000000000000 ) ) ;
#5614 = CARTESIAN_POINT ( 'NONE',  ( 2.121784821874994176, -29.88969486959749844, -11.99819291526277532 ) ) ;
#5615 = FACE_OUTER_BOUND ( 'NONE', #14074, .T. ) ;
#5616 = DIRECTION ( 'NONE',  ( -1.000000000000000000, 0.000000000000000000, 4.336808689942021680E-16 ) ) ;
#5617 = LINE ( 'NONE', #18166, #3775 ) ;
#5618 = CARTESIAN_POINT ( 'NONE',  ( 4.243569643749996345, -28.09038562974308562, -11.56425806667268752 ) ) ;
#5619 = ORIENTED_EDGE ( 'NONE', *, *, #10156, .F. ) ;
#5620 = DIRECTION ( 'NONE',  ( -0.000000000000000000, -1.000000000000000000, -0.000000000000000000 ) ) ;
#5621 = CARTESIAN_POINT ( 'NONE',  ( -2.000000000000005773, -24.77518550192588620, -5.061674863202877184 ) ) ;
#5622 = AXIS2_PLACEMENT_3D ( 'NONE', #412, #7438, #14697 ) ;
#5623 = CARTESIAN_POINT ( 'NONE',  ( 2.864755990943265829, 36.99680007765648071, 2.011557305968487697 ) ) ;
#5624 = PRODUCT_DEFINITION_CONTEXT ( 'detailed design', #6653, 'design' ) ;
#5625 = ORIENTED_EDGE ( 'NONE', *, *, #15651, .F. ) ;
#5626 = CYLINDRICAL_SURFACE ( 'NONE', #1267, 0.9999999999999991118 ) ;
#5627 = AXIS2_PLACEMENT_3D ( 'NONE', #8566, #13021, #13116 ) ;
#5628 = UNCERTAINTY_MEASURE_WITH_UNIT (LENGTH_MEASURE( 1.000000000000000082E-05 ), #5420, 'distance_accuracy_value', 'NONE');
#5629 = CARTESIAN_POINT ( 'NONE',  ( -1.734723475976807094E-15, 40.79999999999999716, -11.50000000000000178 ) ) ;
#5630 = CARTESIAN_POINT ( 'NONE',  ( -0.05938372350921170689, 36.37819992234354771, 2.628655560595669183 ) ) ;
#5631 =( BOUNDED_SURFACE ( )  B_SPLINE_SURFACE ( 3, 2, ( 
 ( #14199, #7138, #12800 ),
 ( #2982, #8613, #17655 ),
 ( #5095, #9271, #7971 ),
 ( #9358, #14954, #667 ),
 ( #13355, #14765, #16429 ),
 ( #7873, #9001, #10753 ),
 ( #15034, #758, #5007 ),
 ( #7599, #16242, #13257 ),
 ( #6218, #13444, #3537 ),
 ( #2337, #10662, #6312 ),
 ( #16155, #4735, #3623 ),
 ( #12137, #10382, #577 ),
 ( #17744, #11866, #14861 ),
 ( #17560, #9181, #476 ),
 ( #17466, #9086, #3447 ),
 ( #2065, #2248, #10568 ),
 ( #11963, #848, #4917 ),
 ( #6120, #6492, #16333 ) ),
 .UNSPECIFIED., .F., .F., .T. ) 
 B_SPLINE_SURFACE_WITH_KNOTS ( ( 4, 2, 2, 2, 2, 2, 2, 2, 4 ),
 ( 3, 3 ),
 ( 2.111895852752043279, 2.369320052961480627, 2.626744253170918419, 2.884168453380356212, 3.141592653589794004, 3.399016853799231797, 3.656441054008669145, 3.913865254218106493, 4.171289454427544285 ),
 ( 0.000000000000000000, 1.000000000000000000 ),
 .UNSPECIFIED. ) 
 GEOMETRIC_REPRESENTATION_ITEM ( )  RATIONAL_B_SPLINE_SURFACE ( (
 ( 1.000000000000000000, 0.8431867568967628124, 1.000000000000000000),
 ( 1.000000000000000000, 0.8610519948705480653, 1.000000000000000000),
 ( 1.000000000000000000, 0.8769588753629522504, 1.000000000000000000),
 ( 1.000000000000000000, 0.9044902796583812465, 1.000000000000000000),
 ( 1.000000000000000000, 0.9161132904341801053, 1.000000000000000000),
 ( 1.000000000000000000, 0.9348125421780860700, 1.000000000000000000),
 ( 1.000000000000000000, 0.9418889734927624602, 1.000000000000000000),
 ( 1.000000000000000000, 0.9513411404402907223, 1.000000000000000000),
 ( 1.000000000000000000, 0.9537169507482278208, 1.000000000000000000),
 ( 1.000000000000000000, 0.9537169507482278208, 1.000000000000000000),
 ( 1.000000000000000000, 0.9513411404402374316, 1.000000000000000000),
 ( 1.000000000000000000, 0.9418889734928156399, 1.000000000000000000),
 ( 1.000000000000000000, 0.9348125421780860700, 1.000000000000000000),
 ( 1.000000000000000000, 0.9161132904341801053, 1.000000000000000000),
 ( 1.000000000000000000, 0.9044902796583805804, 1.000000000000000000),
 ( 1.000000000000000000, 0.8769588753629515843, 1.000000000000000000),
 ( 1.000000000000000000, 0.8610519948705490645, 1.000000000000000000),
 ( 1.000000000000000000, 0.8431867568967623683, 1.000000000000000000) ) ) 
 REPRESENTATION_ITEM ( '' )  SURFACE ( )  );
#5632 = EDGE_LOOP ( 'NONE', ( #5492, #13247, #12663, #3239 ) ) ;
#5633 = CARTESIAN_POINT ( 'NONE',  ( 4.243569643749997233, -28.12264930428783671, -11.61033536916394304 ) ) ;
#5634 = CARTESIAN_POINT ( 'NONE',  ( -4.481649420246366589, 32.87180007765647360, 1.518615910253458878 ) ) ;
#5635 = VERTEX_POINT ( 'NONE', #2096 ) ;
#5636 = SURFACE_STYLE_USAGE ( .BOTH. , #7105 ) ;
#5637 = CARTESIAN_POINT ( 'NONE',  ( -5.577813053751546416E-15, -28.80619019206536535, -9.884235854727139170 ) ) ;
#5638 = VECTOR ( 'NONE', #14121, 1000.000000000000000 ) ;
#5639 = DIRECTION ( 'NONE',  ( 0.000000000000000000, 0.000000000000000000, -1.000000000000000000 ) ) ;
#5640 = CARTESIAN_POINT ( 'NONE',  ( -2.121784821874996396, -20.15854069044762298, -10.91513480593371987 ) ) ;
#5641 = VERTEX_POINT ( 'NONE', #14893 ) ;
#5642 = CARTESIAN_POINT ( 'NONE',  ( 0.000000000000000000, 43.00000000000000000, 0.000000000000000000 ) ) ;
#5643 = VERTEX_POINT ( 'NONE', #2189 ) ;
#5644 = CARTESIAN_POINT ( 'NONE',  ( 3.999999999999996447, -26.08776741350315476, -8.949395057446990265 ) ) ;
#5645 = CARTESIAN_POINT ( 'NONE',  ( -1.071796769724477238, -23.65552896562483198, -2.528329290782095118 ) ) ;
#5646 = CARTESIAN_POINT ( 'NONE',  ( -2.000000000000005773, -28.58229909750097875, -10.49879655616431506 ) ) ;
#5647 = CARTESIAN_POINT ( 'NONE',  ( 1.336863392178569754, 16.25319992234354416, 4.297206761780648421 ) ) ;
#5648 = CARTESIAN_POINT ( 'NONE',  ( 2.211161402132839182, 17.87819992234354771, -2.942372952327217739 ) ) ;
#5649 = EDGE_CURVE ( 'NONE', #6012, #2199, #7447, .T. ) ;
#5650 = CARTESIAN_POINT ( 'NONE',  ( -2.000000000000005773, -29.16304524001135334, -11.32818800201368781 ) ) ;
#5651 = CARTESIAN_POINT ( 'NONE',  ( -0.7188294034286043521, 39.99680007765647360, 2.395093729190366005 ) ) ;
#5652 = CARTESIAN_POINT ( 'NONE',  ( 4.499999999999999112, 33.25319992234354771, 0.05647727720528474687 ) ) ;
#5653 = CARTESIAN_POINT ( 'NONE',  ( 4.713407268011036227E-15, -19.48762356985234945, -11.60236650416142723 ) ) ;
#5654 = ORIENTED_EDGE ( 'NONE', *, *, #17359, .T. ) ;
#5655 = CARTESIAN_POINT ( 'NONE',  ( 1.071796769724476128, -17.48947670584981751, -7.669868411485510684 ) ) ;
#5656 =( BOUNDED_CURVE ( )  B_SPLINE_CURVE ( 2, ( #2088, #17490, #7718, #16086, #1805, #3379, #7811, #15991, #14884 ),
 .UNSPECIFIED., .F., .T. ) 
 B_SPLINE_CURVE_WITH_KNOTS ( ( 3, 2, 2, 2, 3 ),
 ( 0.1982758620689655249, 0.2011494252873563260, 0.2068965517241379282, 0.2126436781609195303, 0.2155172413793103592 ),
 .UNSPECIFIED. ) 
 CURVE ( )  GEOMETRIC_REPRESENTATION_ITEM ( )  RATIONAL_B_SPLINE_CURVE ( ( 0.9330127018922194093, 0.9330127018922194093, 1.000000000000000000, 0.8660254037844387076, 1.000000000000000000, 0.8660254037844387076, 1.000000000000000000, 0.9330127018922189652, 0.9330127018922192983 ) ) 
 REPRESENTATION_ITEM ( '' )  );
#5657 = CARTESIAN_POINT ( 'NONE',  ( 2.864755990943265829, 24.49680007765647716, 2.011557305968487697 ) ) ;
#5658 = CARTESIAN_POINT ( 'NONE',  ( -8.999999999999998224, -10.00000000000000178, 15.14468620625656747 ) ) ;
#5659 = CARTESIAN_POINT ( 'NONE',  ( 4.243569643749997233, -24.73496347708949017, -6.772218607582066952 ) ) ;
#5660 = CARTESIAN_POINT ( 'NONE',  ( -3.673772985318219053, 25.74680007765648426, -2.599342558260952174 ) ) ;
#5661 =( GEOMETRIC_REPRESENTATION_CONTEXT ( 3 ) GLOBAL_UNCERTAINTY_ASSIGNED_CONTEXT ( ( #13821 ) ) GLOBAL_UNIT_ASSIGNED_CONTEXT ( ( #14889, #603, #6243 ) ) REPRESENTATION_CONTEXT ( 'NONE', 'WORKASPACE' ) );
#5662 = CARTESIAN_POINT ( 'NONE',  ( -4.000000000000004441, -26.69002267167174125, -9.809504703950439719 ) ) ;
#5663 = DIRECTION ( 'NONE',  ( 0.000000000000000000, 0.000000000000000000, -1.000000000000000000 ) ) ;
#5664 = VERTEX_POINT ( 'NONE', #13474 ) ;
#5665 = ORIENTED_EDGE ( 'NONE', *, *, #520, .F. ) ;
#5666 = CARTESIAN_POINT ( 'NONE',  ( 1.135272562821090458, 24.74680007765647716, 3.311245368580554072 ) ) ;
#5667 = FACE_OUTER_BOUND ( 'NONE', #867, .T. ) ;
#5668 = CARTESIAN_POINT ( 'NONE',  ( -13.00000000000000178, 15.00000000000000178, -16.00000000000000000 ) ) ;
#5669 = CARTESIAN_POINT ( 'NONE',  ( 0.000000000000000000, -1.759474945355388176, -3.047499999999998099 ) ) ;
#5670 =( NAMED_UNIT ( * ) PLANE_ANGLE_UNIT ( ) SI_UNIT ( $, .RADIAN. ) );
#5671 = ORIENTED_EDGE ( 'NONE', *, *, #11683, .F. ) ;
#5672 = CARTESIAN_POINT ( 'NONE',  ( 2.798362969681409851, 21.00319992234354416, 2.102939460078764977 ) ) ;
#5673 = CARTESIAN_POINT ( 'NONE',  ( -4.243569643749997233, -21.10823983395705383, -10.13570068892072840 ) ) ;
#5674 = CARTESIAN_POINT ( 'NONE',  ( 0.7188294034286049072, 16.24680007765648071, -2.395093729190366005 ) ) ;
#5675 = CARTESIAN_POINT ( 'NONE',  ( 3.518350579753605434, 38.12819992234354061, -1.080741659609877114 ) ) ;
#5676 = AXIS2_PLACEMENT_3D ( 'NONE', #9653, #18037, #13553 ) ;
#5677 = CARTESIAN_POINT ( 'NONE',  ( 3.579096709490575479E-14, -24.41833045397989821, -3.617722715916328546 ) ) ;
#5678 = DIRECTION ( 'NONE',  ( 3.469446951953612217E-16, -0.000000000000000000, 1.000000000000000000 ) ) ;
#5679 = STYLED_ITEM ( 'NONE', ( #9793 ), #16698 ) ;
#5680 = CARTESIAN_POINT ( 'NONE',  ( 2.121784821874994176, -25.53409880605677884, -5.777757078943218438 ) ) ;
#5681 = ADVANCED_FACE ( 'NONE', ( #7540 ), #15998, .T. ) ;
#5682 = EDGE_CURVE ( 'NONE', #9202, #10567, #8102, .T. ) ;
#5683 = DIRECTION ( 'NONE',  ( -0.000000000000000000, -1.000000000000000000, -0.000000000000000000 ) ) ;
#5684 = LINE ( 'NONE', #3182, #6227 ) ;
#5685 = VECTOR ( 'NONE', #10961, 1000.000000000000000 ) ;
#5686 = CARTESIAN_POINT ( 'NONE',  ( -5.577813053751546416E-15, -24.16022105762192851, -3.249104295986281699 ) ) ;
#5687 = CARTESIAN_POINT ( 'NONE',  ( 4.243569643749996345, -23.18630709894168263, -4.560508088001781424 ) ) ;
#5688 = LINE ( 'NONE', #8828, #11825 ) ;
#5690 = DIRECTION ( 'NONE',  ( -1.000000000000000000, 0.000000000000000000, 0.000000000000000000 ) ) ;
#5689 = PRODUCT_DEFINITION_FORMATION_WITH_SPECIFIED_SOURCE ( 'ANY', '', #8117, .NOT_KNOWN. ) ;
#5691 = ADVANCED_FACE ( 'NONE', ( #16095 ), #9027, .T. ) ;
#5692 = ORIENTED_EDGE ( 'NONE', *, *, #15002, .T. ) ;
#5693 = CARTESIAN_POINT ( 'NONE',  ( -2.481649420246391902, 22.12819992234354771, -0.8687765177875723666 ) ) ;
#5694 = DIRECTION ( 'NONE',  ( 1.000000000000000000, 0.000000000000000000, 0.000000000000000000 ) ) ;
#5695 = CARTESIAN_POINT ( 'NONE',  ( -8.000000000000001776, 18.79999999999999361, 2.499999999999998224 ) ) ;
#5696 = CARTESIAN_POINT ( 'NONE',  ( -1.734723475976807094E-15, 40.79999999999999716, -2.500000000000000000 ) ) ;
#5697 = CARTESIAN_POINT ( 'NONE',  ( -15.00000000000000178, 13.00000000000000178, 24.99999999999999645 ) ) ;
#5698 = ORIENTED_EDGE ( 'NONE', *, *, #7710, .F. ) ;
#5699 = AXIS2_PLACEMENT_3D ( 'NONE', #12027, #10641, #3600 ) ;
#5700 = CARTESIAN_POINT ( 'NONE',  ( 2.121784821875004390, -17.10424616687832966, -6.553150170094818705 ) ) ;
#5701 = CARTESIAN_POINT ( 'NONE',  ( -3.481649420246369697, 32.87180007765645939, 1.193696214020542490 ) ) ;
#5702 = AXIS2_PLACEMENT_3D ( 'NONE', #15946, #17639, #1857 ) ;
#5703 = CARTESIAN_POINT ( 'NONE',  ( 8.500000000000019540, 0.000000000000000000, -20.49999999999998934 ) ) ;
#5704 = EDGE_CURVE ( 'NONE', #6724, #3078, #17309, .T. ) ;
#5705 = AXIS2_PLACEMENT_3D ( 'NONE', #4971, #10444, #16121 ) ;
#5706 = CARTESIAN_POINT ( 'NONE',  ( 4.730628863548789710E-15, -22.24162695414431568, -16.02583535712476959 ) ) ;
#5707 = LINE ( 'NONE', #17221, #6416 ) ;
#5708 = DIRECTION ( 'NONE',  ( 1.049727191973305394E-16, 0.5150380737757255245, -0.8571673013836856869 ) ) ;
#5709 = CARTESIAN_POINT ( 'NONE',  ( 8.000000000000000000, 0.000000000000000000, -4.400000000000002132 ) ) ;
#5710 = CARTESIAN_POINT ( 'NONE',  ( -4.243569643750000786, -24.90044036093436119, -11.28003420104843357 ) ) ;
#5711 = ORIENTED_EDGE ( 'NONE', *, *, #11064, .T. ) ;
#5712 = CARTESIAN_POINT ( 'NONE',  ( 14.99999999999999822, 10.00000000000000000, 24.99999999999999645 ) ) ;
#5713 = VECTOR ( 'NONE', #15082, 1000.000000000000114 ) ;
#5714 = CARTESIAN_POINT ( 'NONE',  ( 4.000000000000000888, -20.56097613501849608, -5.082637016477885794 ) ) ;
#5715 = MECHANICAL_DESIGN_GEOMETRIC_PRESENTATION_REPRESENTATION (  '', ( #6603 ), #14001 ) ;
#5716 = CARTESIAN_POINT ( 'NONE',  ( 0.05938372350926800214, 22.37180007765647716, 2.628655560595669183 ) ) ;
#5717 = EDGE_LOOP ( 'NONE', ( #17976, #15950, #16496, #11724 ) ) ;
#5718 = CARTESIAN_POINT ( 'NONE',  ( -4.648177544792955347E-16, -30.09673717385520675, -11.72732795437737785 ) ) ;
#5719 = CARTESIAN_POINT ( 'NONE',  ( -1.999999999999996225, -20.21840771348061949, -10.63287546870361666 ) ) ;
#5720 = CARTESIAN_POINT ( 'NONE',  ( 2.518350579753611207, 38.12819992234354771, -0.7558219633769606149 ) ) ;
#5721 = ORIENTED_EDGE ( 'NONE', *, *, #13575, .T. ) ;
#5722 = CARTESIAN_POINT ( 'NONE',  ( 4.243569643750000786, -24.80364933730013277, -11.14180229357466345 ) ) ;
#5723 = CARTESIAN_POINT ( 'NONE',  ( 1.336863392178479160, 36.24680007765647360, -4.297206761780677731 ) ) ;
#5724 = ADVANCED_FACE ( 'NONE', ( #6433 ), #4256, .T. ) ;
#5725 = VERTEX_POINT ( 'NONE', #3475 ) ;
#5726 = CIRCLE ( 'NONE', #10465, 3.000000000000000444 ) ;
#5727 = CARTESIAN_POINT ( 'NONE',  ( 1.999999999999994449, -22.92540149469378363, -2.419909520370864264 ) ) ;
#5728 = CARTESIAN_POINT ( 'NONE',  ( 1.999999999999994449, -24.15142112668919339, -4.170847014031824784 ) ) ;
#5729 = DIRECTION ( 'NONE',  ( -3.373073425510457965E-16, 0.000000000000000000, -1.000000000000000000 ) ) ;
#5730 = CARTESIAN_POINT ( 'NONE',  ( 0.000000000000000000, -0.7216878364870317197, 1.250000000000000000 ) ) ;
#5731 = CARTESIAN_POINT ( 'NONE',  ( 2.121784821874994176, -24.50166122062490359, -4.303283399223027494 ) ) ;
#5732 = ORIENTED_EDGE ( 'NONE', *, *, #6928, .F. ) ;
#5733 = CARTESIAN_POINT ( 'NONE',  ( -5.577813053751546416E-15, -26.41867827504920996, -6.474515469367432274 ) ) ;
#5734 = ORIENTED_EDGE ( 'NONE', *, *, #4354, .F. ) ;
#5735 = ORIENTED_EDGE ( 'NONE', *, *, #6017, .F. ) ;
#5736 =( BOUNDED_CURVE ( )  B_SPLINE_CURVE ( 2, ( #3894, #8247, #5377, #3796, #13908, #9543, #12231, #6581, #11026, #5465, #13718, #16800, #13532, #17919, #9453, #2429, #8150, #1123, #12416, #16707, #17419, #4687, #15730, #11821, #7368, #5799, #17517, #15826, #14339, #1735, #13028, #344, #11725, #3122, #10240, #245, #5981, #6071, #8756, #12845, #2938, #15917, #11634, #8573, #17328, #14430, #14246, #8851, #10335, #4591, #1549, #7187, #11443, #4504, #17135, #15406, #13210, #3218, #14531, #16014, #10147, #1828, #6173, #4411, #7465, #9719, #3306, #149, #5890, #12930, #13124, #11539, #8948, #433, #14629, #1931, #7555, #527, #17231, #10053, #3028, #8662, #1637, #7274, #14815, #3754, #3579, #2292, #9229, #801, #9044, #16111, #4962, #624, #9136, #6537, #13669, #10525, #989, #16197, #9403, #13311, #7743, #13487, #6361, #16384, #17612, #3488, #12189, #12003, #17876, #2113, #17792, #2205, #5145, #7921, #17698, #16473, #12096, #13401, #14720, #4779, #2018, #15081, #7646, #6633, #713, #10803, #10431, #7831, #3402, #5052, #6263, #10708, #2385, #10618, #12278, #6448, #11915, #4874, #16292, #8016, #14911, #3673, #9318, #14991, #13578, #895, #5424, #3850, #13861, #6982, #16846, #9676, #18240, #8292, #5334, #14130, #4029, #5510, #16939, #2477, #11156, #15173, #2567, #1442, #8198, #1169, #16755, #6809, #7072, #18333, #4124, #12459, #3940, #10985, #17967, #15358, #5236, #1350, #16664, #9496, #10891, #18154, #13766, #9591, #12643, #8462, #15269, #16570, #11072, #4212, #12367, #8107, #2657, #13950, #1263, #9772, #18061, #6895, #5606 ),
 .UNSPECIFIED., .F., .T. ) 
 B_SPLINE_CURVE_WITH_KNOTS ( ( 3, 2, 2, 2, 2, 2, 2, 2, 2, 2, 2, 2, 2, 2, 2, 2, 2, 2, 2, 2, 2, 2, 2, 2, 2, 2, 2, 2, 2, 2, 2, 2, 2, 2, 2, 2, 2, 2, 2, 2, 2, 2, 2, 2, 2, 2, 2, 2, 2, 2, 2, 2, 2, 2, 2, 2, 2, 2, 2, 2, 2, 2, 2, 2, 2, 2, 2, 2, 2, 2, 2, 2, 2, 2, 2, 2, 2, 2, 2, 2, 2, 2, 2, 2, 2, 2, 2, 2, 2, 2, 2, 2, 2, 2, 2, 2, 2, 2, 2, 2, 3 ),
 ( 0.000000000000000000, 0.01000000000000000021, 0.02000000000000000042, 0.02999999999999999889, 0.04000000000000000083, 0.05000000000000000278, 0.05999999999999999778, 0.07000000000000000666, 0.08000000000000000167, 0.08999999999999999667, 0.1000000000000000056, 0.1100000000000000006, 0.1199999999999999956, 0.1300000000000000044, 0.1400000000000000133, 0.1499999999999999944, 0.1600000000000000033, 0.1700000000000000122, 0.1799999999999999933, 0.1900000000000000022, 0.2000000000000000111, 0.2099999999999999922, 0.2200000000000000011, 0.2300000000000000100, 0.2399999999999999911, 0.2500000000000000000, 0.2600000000000000089, 0.2700000000000000178, 0.2800000000000000266, 0.2899999999999999800, 0.2999999999999999889, 0.3099999999999999978, 0.3200000000000000067, 0.3300000000000000155, 0.3400000000000000244, 0.3499999999999999778, 0.3599999999999999867, 0.3699999999999999956, 0.3800000000000000044, 0.3900000000000000133, 0.4000000000000000222, 0.4099999999999999756, 0.4199999999999999845, 0.4299999999999999933, 0.4400000000000000022, 0.4500000000000000111, 0.4600000000000000200, 0.4699999999999999734, 0.4799999999999999822, 0.4899999999999999911, 0.5000000000000000000, 0.5100000000000000089, 0.5200000000000000178, 0.5300000000000000266, 0.5400000000000000355, 0.5500000000000000444, 0.5600000000000000533, 0.5699999999999999512, 0.5799999999999999600, 0.5899999999999999689, 0.5999999999999999778, 0.6099999999999999867, 0.6199999999999999956, 0.6300000000000000044, 0.6400000000000000133, 0.6500000000000000222, 0.6600000000000000311, 0.6700000000000000400, 0.6800000000000000488, 0.6899999999999999467, 0.6999999999999999556, 0.7099999999999999645, 0.7199999999999999734, 0.7299999999999999822, 0.7399999999999999911, 0.7500000000000000000, 0.7600000000000000089, 0.7700000000000000178, 0.7800000000000000266, 0.7900000000000000355, 0.8000000000000000444, 0.8100000000000000533, 0.8199999999999999512, 0.8299999999999999600, 0.8399999999999999689, 0.8499999999999999778, 0.8599999999999999867, 0.8699999999999999956, 0.8800000000000000044, 0.8900000000000000133, 0.9000000000000000222, 0.9100000000000000311, 0.9200000000000000400, 0.9300000000000000488, 0.9399999999999999467, 0.9499999999999999556, 0.9599999999999999645, 0.9699999999999999734, 0.9799999999999999822, 0.9899999999999999911, 1.000000000000000000 ),
 .UNSPECIFIED. ) 
 CURVE ( )  GEOMETRIC_REPRESENTATION_ITEM ( )  RATIONAL_B_SPLINE_CURVE ( ( 1.000000000000000000, 0.9510565162951535312, 1.000000000000000000, 0.9510565162951535312, 1.000000000000000000, 0.9510565162951535312, 1.000000000000000000, 0.9510565162951535312, 1.000000000000000000, 0.9510565162951535312, 1.000000000000000000, 0.9510565162951535312, 1.000000000000000000, 0.9510565162951535312, 1.000000000000000000, 0.9510565162951535312, 1.000000000000000000, 0.9510565162951535312, 1.000000000000000000, 0.9510565162951535312, 1.000000000000000000, 0.9510565162951535312, 1.000000000000000000, 0.9510565162951535312, 1.000000000000000000, 0.9510565162951535312, 1.000000000000000000, 0.9510565162951535312, 1.000000000000000000, 0.9510565162951535312, 1.000000000000000000, 0.9510565162951535312, 1.000000000000000000, 0.9510565162951535312, 1.000000000000000000, 0.9510565162951535312, 1.000000000000000000, 0.9510565162951535312, 1.000000000000000000, 0.9510565162951535312, 1.000000000000000000, 0.9510565162951535312, 1.000000000000000000, 0.9510565162951535312, 1.000000000000000000, 0.9510565162951535312, 1.000000000000000000, 0.9510565162951535312, 1.000000000000000000, 0.9510565162951535312, 1.000000000000000000, 0.9510565162951535312, 1.000000000000000000, 0.9510565162951535312, 1.000000000000000000, 0.9510565162951535312, 1.000000000000000000, 0.9510565162951535312, 1.000000000000000000, 0.9510565162951535312, 1.000000000000000000, 0.9510565162951535312, 1.000000000000000000, 0.9510565162951535312, 1.000000000000000000, 0.9510565162951535312, 1.000000000000000000, 0.9510565162951535312, 1.000000000000000000, 0.9510565162951535312, 1.000000000000000000, 0.9510565162951535312, 1.000000000000000000, 0.9510565162951535312, 1.000000000000000000, 0.9510565162951535312, 1.000000000000000000, 0.9510565162951535312, 1.000000000000000000, 0.9510565162951535312, 1.000000000000000000, 0.9510565162951535312, 1.000000000000000000, 0.9510565162951535312, 1.000000000000000000, 0.9510565162951535312, 1.000000000000000000, 0.9510565162951535312, 1.000000000000000000, 0.9510565162951535312, 1.000000000000000000, 0.9510565162951535312, 1.000000000000000000, 0.9510565162951535312, 1.000000000000000000, 0.9510565162951535312, 1.000000000000000000, 0.9510565162951535312, 1.000000000000000000, 0.9510565162951535312, 1.000000000000000000, 0.9510565162951535312, 1.000000000000000000, 0.9510565162951535312, 1.000000000000000000, 0.9510565162951535312, 1.000000000000000000, 0.9510565162951535312, 1.000000000000000000, 0.9510565162951535312, 1.000000000000000000, 0.9510565162951535312, 1.000000000000000000, 0.9510565162951535312, 1.000000000000000000, 0.9510565162951535312, 1.000000000000000000, 0.9510565162951535312, 1.000000000000000000, 0.9510565162951535312, 1.000000000000000000, 0.9510565162951535312, 1.000000000000000000, 0.9510565162951535312, 1.000000000000000000, 0.9510565162951535312, 1.000000000000000000, 0.9510565162951535312, 1.000000000000000000, 0.9510565162951535312, 1.000000000000000000, 0.9510565162951535312, 1.000000000000000000, 0.9510565162951535312, 1.000000000000000000, 0.9510565162951535312, 1.000000000000000000, 0.9510565162951535312, 1.000000000000000000, 0.9510565162951535312, 1.000000000000000000, 0.9510565162951535312, 1.000000000000000000, 0.9510565162951535312, 1.000000000000000000, 0.9510565162951535312, 1.000000000000000000, 0.9510565162951535312, 1.000000000000000000, 0.9510565162951535312, 1.000000000000000000, 0.9510565162951535312, 1.000000000000000000, 0.9510565162951535312, 1.000000000000000000, 0.9510565162951535312, 1.000000000000000000, 0.9510565162951535312, 1.000000000000000000, 0.9510565162951535312, 1.000000000000000000, 0.9510565162951535312, 1.000000000000000000, 0.9510565162951535312, 1.000000000000000000, 0.9510565162951535312, 1.000000000000000000, 0.9510565162951535312, 1.000000000000000000, 0.9510565162951535312, 1.000000000000000000, 0.9510565162951535312, 1.000000000000000000, 0.9510565162951535312, 1.000000000000000000, 0.9510565162951535312, 1.000000000000000000, 0.9510565162951535312, 1.000000000000000000, 0.9510565162951535312, 1.000000000000000000, 0.9510565162951535312, 1.000000000000000000, 0.9510565162951535312, 1.000000000000000000, 0.9510565162951535312, 1.000000000000000000, 0.9510565162951535312, 1.000000000000000000, 0.9510565162951535312, 1.000000000000000000, 0.9510565162951535312, 1.000000000000000000, 0.9510565162951535312, 1.000000000000000000, 0.9510565162951535312, 1.000000000000000000, 0.9510565162951535312, 1.000000000000000000, 0.9510565162951535312, 1.000000000000000000 ) ) 
 REPRESENTATION_ITEM ( '' )  );
#5737 = DIRECTION ( 'NONE',  ( 0.000000000000000000, 0.000000000000000000, 1.000000000000000000 ) ) ;
#5738 = CIRCLE ( 'NONE', #10475, 4.000000000000001776 ) ;
#5739 = CARTESIAN_POINT ( 'NONE',  ( 2.399999999999999911, 0.000000000000000000, 0.000000000000000000 ) ) ;
#5740 = CARTESIAN_POINT ( 'NONE',  ( -0.05938372350918959958, 18.87819992234354416, 4.731580009072201776 ) ) ;
#5741 = CARTESIAN_POINT ( 'NONE',  ( 1.027846397803612311, 31.25319992234354416, 3.346150245485499219 ) ) ;
#5742 = CARTESIAN_POINT ( 'NONE',  ( -2.000000000000005773, -29.42115463636932304, -11.69680642194373554 ) ) ;
#5743 = CARTESIAN_POINT ( 'NONE',  ( -0.05938372350926768989, 36.12180007765648071, -2.628655560595669183 ) ) ;
#5744 = CARTESIAN_POINT ( 'NONE',  ( -4.481649420246396787, 37.12819992234354061, -1.518615910253363399 ) ) ;
#5745 = CARTESIAN_POINT ( 'NONE',  ( 4.000000000000003553, -21.93861120840455214, -11.07642170763079292 ) ) ;
#5746 = ORIENTED_EDGE ( 'NONE', *, *, #7254, .T. ) ;
#5747 = EDGE_CURVE ( 'NONE', #2227, #1500, #4946, .T. ) ;
#5748 = AXIS2_PLACEMENT_3D ( 'NONE', #5543, #1112, #5370 ) ;
#5749 = DIRECTION ( 'NONE',  ( 0.000000000000000000, 0.000000000000000000, 1.000000000000000000 ) ) ;
#5750 = CARTESIAN_POINT ( 'NONE',  ( -2.211161402132902243, 20.87180007765647716, -2.942372952327172886 ) ) ;
#5751 = ADVANCED_FACE ( 'NONE', ( #11059 ), #18044, .T. ) ;
#5752 = CARTESIAN_POINT ( 'NONE',  ( 9.000000000000005329, -10.00000000000000000, 15.14468620625654616 ) ) ;
#5753 = CARTESIAN_POINT ( 'NONE',  ( -4.243569643750004339, -25.33721873525807666, -7.632328254085517294 ) ) ;
#5754 = ADVANCED_FACE ( 'NONE', ( #4017 ), #2464, .F. ) ;
#5755 = CARTESIAN_POINT ( 'NONE',  ( 3.607379964056306676, 23.99680007765647716, -2.690724712371305838 ) ) ;
#5756 = LINE ( 'NONE', #17348, #8903 ) ;
#5757 = LINE ( 'NONE', #3069, #8836 ) ;
#5758 = VERTEX_POINT ( 'NONE', #5127 ) ;
#5759 = ORIENTED_EDGE ( 'NONE', *, *, #2652, .T. ) ;
#5760 = CARTESIAN_POINT ( 'NONE',  ( -2.864755990943265829, 23.24680007765647716, -2.011557305968488141 ) ) ;
#5761 = FACE_OUTER_BOUND ( 'NONE', #8478, .T. ) ;
#5762 = CARTESIAN_POINT ( 'NONE',  ( 5.759474945355412601, 0.000000000000000000, 0.000000000000000000 ) ) ;
#5763 = EDGE_LOOP ( 'NONE', ( #12953, #18129, #643, #949 ) ) ;
#5764 = CARTESIAN_POINT ( 'NONE',  ( 2.211161402132839626, 15.37819992234354771, -2.942372952327218183 ) ) ;
#5765 = CARTESIAN_POINT ( 'NONE',  ( -4.243569643749997233, -20.59202104124112154, -9.398463849060638253 ) ) ;
#5766 = CARTESIAN_POINT ( 'NONE',  ( 1.135272562821090458, 37.24680007765648071, 3.311245368580554072 ) ) ;
#5767 = CARTESIAN_POINT ( 'NONE',  ( -0.05938372350920063936, 36.37819992234355482, 3.680117784833935701 ) ) ;
#5768 = DIRECTION ( 'NONE',  ( 0.000000000000000000, 0.000000000000000000, -1.000000000000000000 ) ) ;
#5769 = CARTESIAN_POINT ( 'NONE',  ( 1.071796769724494780, -28.27844469863059018, -9.130537180211129922 ) ) ;
#5770 = CARTESIAN_POINT ( 'NONE',  ( -4.243569643750000786, -22.35161007189942595, -7.639927304239214401 ) ) ;
#5771 = CARTESIAN_POINT ( 'NONE',  ( -4.242943609565101859, -15.02914320863489550, -7.979206348032058749 ) ) ;
#5772 = CARTESIAN_POINT ( 'NONE',  ( 0.3999999999999975797, 0.000000000000000000, 0.000000000000000000 ) ) ;
#5773 = CARTESIAN_POINT ( 'NONE',  ( -5.577813053751546416E-15, -23.32136551875358421, -2.051094430206859887 ) ) ;
#5774 = CARTESIAN_POINT ( 'NONE',  ( -2.121784821874996396, -17.80329244868115168, -7.551491724072033840 ) ) ;
#5775 = FACE_OUTER_BOUND ( 'NONE', #6105, .T. ) ;
#5776 = CARTESIAN_POINT ( 'NONE',  ( -1.734723475976807094E-15, 27.59999999999999432, -11.50000000000000178 ) ) ;
#5777 = VERTEX_POINT ( 'NONE', #3925 ) ;
#5778 = CARTESIAN_POINT ( 'NONE',  ( -2.518350579753611207, 24.37819992234354416, 0.7558219633769609480 ) ) ;
#5779 = CARTESIAN_POINT ( 'NONE',  ( -1.734723475976807094E-15, 31.99999999999999289, -2.500000000000000000 ) ) ;
#5780 = CARTESIAN_POINT ( 'NONE',  ( 1.027846397803542144, 16.24680007765647716, -3.346150245485522312 ) ) ;
#5781 = DIRECTION ( 'NONE',  ( 0.000000000000000000, 0.000000000000000000, -1.000000000000000000 ) ) ;
#5782 = CARTESIAN_POINT ( 'NONE',  ( 4.000000000000000000, 3.518949890710770134, -4.119968255444916849E-15 ) ) ;
#5783 = EDGE_CURVE ( 'NONE', #10810, #7195, #9662, .T. ) ;
#5784 = ORIENTED_EDGE ( 'NONE', *, *, #7209, .T. ) ;
#5785 = CARTESIAN_POINT ( 'NONE',  ( -2.121784821875005722, -23.51224186791935011, -2.890246122824515318 ) ) ;
#5786 = CARTESIAN_POINT ( 'NONE',  ( 2.211161402132902243, 29.62180007765648071, 2.942372952327172442 ) ) ;
#5787 = CARTESIAN_POINT ( 'NONE',  ( 4.243569643750003451, -24.84007152296602428, -15.46530867707600088 ) ) ;
#5788 = DIRECTION ( 'NONE',  ( -1.000000000000000000, 0.000000000000000000, 4.336808689942021680E-16 ) ) ;
#5789 = CARTESIAN_POINT ( 'NONE',  ( -4.243569643750000786, -25.67476855000827030, -12.38588946083857856 ) ) ;
#5790 = DIRECTION ( 'NONE',  ( -0.000000000000000000, -1.000000000000000000, -0.000000000000000000 ) ) ;
#5791 = DIRECTION ( 'NONE',  ( 0.000000000000000000, 1.000000000000000000, 0.000000000000000000 ) ) ;
#5792 = DIRECTION ( 'NONE',  ( 0.000000000000000000, 0.000000000000000000, 1.000000000000000000 ) ) ;
#5793 = CONICAL_SURFACE ( 'NONE', #6402, 2.000000000000001776, 1.029744260000000189 ) ;
#5794 = CARTESIAN_POINT ( 'NONE',  ( 2.121784821874994176, -28.34103849144968379, -9.786482395682487123 ) ) ;
#5795 = LINE ( 'NONE', #11438, #7122 ) ;
#5796 = CARTESIAN_POINT ( 'NONE',  ( -3.999999999999997335, -18.04546114737679474, -5.516427208026009055 ) ) ;
#5797 = CARTESIAN_POINT ( 'NONE',  ( -1.989345975306426206, 25.24680007765648071, 1.515154207786343799 ) ) ;
#5798 = ORIENTED_EDGE ( 'NONE', *, *, #10968, .T. ) ;
#5799 = CARTESIAN_POINT ( 'NONE',  ( -0.05938372350927861865, 18.62180007765647716, -3.680117784833935701 ) ) ;
#5800 = CARTESIAN_POINT ( 'NONE',  ( 4.243569643750000786, -27.12663390452184942, -14.45936807294509308 ) ) ;
#5801 = ADVANCED_FACE ( 'NONE', ( #16554 ), #1604, .T. ) ;
#5802 = DIRECTION ( 'NONE',  ( 0.000000000000000000, 0.000000000000000000, 1.000000000000000000 ) ) ;
#5803 = CARTESIAN_POINT ( 'NONE',  ( 8.499999999999994671, 13.00000000000000000, 18.34999999999999787 ) ) ;
#5804 = ADVANCED_FACE ( 'NONE', ( #5039 ), #9301, .T. ) ;
#5805 = CARTESIAN_POINT ( 'NONE',  ( -2.518350579753611207, 34.37819992234354771, 0.7558219633769609480 ) ) ;
#5806 = ORIENTED_EDGE ( 'NONE', *, *, #13858, .T. ) ;
#5807 = CARTESIAN_POINT ( 'NONE',  ( -4.243569643750004339, -26.40191999523469946, -9.152879236296964649 ) ) ;
#5808 = EDGE_CURVE ( 'NONE', #8825, #1458, #3832, .T. ) ;
#5809 = CARTESIAN_POINT ( 'NONE',  ( -4.499999999999999112, 35.49680007765647360, 0.05647727720537927543 ) ) ;
#5810 = AXIS2_PLACEMENT_3D ( 'NONE', #17125, #14618, #17411 ) ;
#5811 = ORIENTED_EDGE ( 'NONE', *, *, #1747, .T. ) ;
#5812 = DIRECTION ( 'NONE',  ( 0.000000000000000000, 0.8191520442889952403, -0.5735764363510413855 ) ) ;
#5813 = CARTESIAN_POINT ( 'NONE',  ( 4.000000000000003553, -20.90617362297267690, -9.601948027910603756 ) ) ;
#5814 = CARTESIAN_POINT ( 'NONE',  ( 1.999999999999994449, -24.92574931576309538, -5.276702273821968880 ) ) ;
#5815 = CARTESIAN_POINT ( 'NONE',  ( -3.706921591972381904E-14, -19.73640722255826319, -10.87881775021074127 ) ) ;
#5816 = CARTESIAN_POINT ( 'NONE',  ( 6.428571428571431490, -11.73421655796352425, 14.25837509840157935 ) ) ;
#5817 = CARTESIAN_POINT ( 'NONE',  ( 4.243569643749996345, -22.96046137712846047, -4.237966970562988323 ) ) ;
#5818 = ORIENTED_EDGE ( 'NONE', *, *, #16301, .T. ) ;
#5819 = FACE_OUTER_BOUND ( 'NONE', #3425, .T. ) ;
#5820 = ORIENTED_EDGE ( 'NONE', *, *, #7161, .F. ) ;
#5821 = ORIENTED_EDGE ( 'NONE', *, *, #2645, .T. ) ;
#5822 = CARTESIAN_POINT ( 'NONE',  ( -8.500000000000010658, 13.00000000000000178, 20.49999999999998934 ) ) ;
#5823 = CARTESIAN_POINT ( 'NONE',  ( -4.000000000000004441, -27.65793290730917064, -11.19182377768135161 ) ) ;
#5824 = CARTESIAN_POINT ( 'NONE',  ( 1.336863392178569754, 21.25319992234354771, 4.297206761780648421 ) ) ;
#5825 = CARTESIAN_POINT ( 'NONE',  ( -2.864755990943222308, 31.75319992234354416, 2.011557305968548093 ) ) ;
#5826 = CARTESIAN_POINT ( 'NONE',  ( 1.989345975306426206, 38.99680007765648071, -1.515154207786343799 ) ) ;
#5827 = ORIENTED_EDGE ( 'NONE', *, *, #16209, .F. ) ;
#5828 = CARTESIAN_POINT ( 'NONE',  ( -2.829195390882724315, 34.12819992234354771, 3.793023760679264722 ) ) ;
#5829 = CARTESIAN_POINT ( 'NONE',  ( -4.000000000000000888, -22.94848805062475350, -8.492357399824065567 ) ) ;
#5830 = ORIENTED_EDGE ( 'NONE', *, *, #3989, .F. ) ;
#5831 = CARTESIAN_POINT ( 'NONE',  ( -3.500000000000000444, 40.49680007765648071, 0.05647727720536853402 ) ) ;
#5832 = AXIS2_PLACEMENT_3D ( 'NONE', #3134, #6281, #16129 ) ;
#5833 = CARTESIAN_POINT ( 'NONE',  ( 1.135272562821090458, 32.24680007765648071, 3.311245368580554072 ) ) ;
#5834 = FACE_OUTER_BOUND ( 'NONE', #7747, .T. ) ;
#5835 = CARTESIAN_POINT ( 'NONE',  ( 2.121784821875004390, -18.87874826683935936, -9.087401807113897334 ) ) ;
#5836 = CARTESIAN_POINT ( 'NONE',  ( 0.05938372350929014415, 34.87180007765647360, 4.731580009072201776 ) ) ;
#5837 = DIRECTION ( 'NONE',  ( 0.000000000000000000, 0.000000000000000000, -1.000000000000000000 ) ) ;
#5838 = ORIENTED_EDGE ( 'NONE', *, *, #7896, .T. ) ;
#5839 = VERTEX_POINT ( 'NONE', #12448 ) ;
#5840 = CARTESIAN_POINT ( 'NONE',  ( 0.05938372350927906274, 19.87180007765648426, 3.680117784833935701 ) ) ;
#5841 = CLOSED_SHELL ( 'NONE', ( #16256, #13680, #13353, #8347, #7664, #5275, #1048, #14083, #3278, #5906, #16991, #14251, #3756, #12480, #7056, #9974, #15585, #30, #9862, #7992, #13011, #10103, #15120, #3764, #1928, #3104, #1406, #12430, #17952, #9351, #12248, #6362, #1811, #6547, #16352, #4045, #6675, #8872, #17956, #79, #3043, #17500, #2260, #16716, #840, #6931, #2095, #491, #16151, #11505, #17971, #3386, #7328, #9390, #615, #7604, #5754, #3436, #18357, #10399, #6139, #12717, #12110, #8432, #7833, #9095, #3307, #11645, #8628, #9982, #9140, #1124, #890, #6487, #6769, #267, #18298, #2486, #9934, #5584, #5454, #9030, #715, #17737, #9594, #1284, #6391, #5015, #1963, #9040, #15295, #18363, #15167, #1669, #3884, #17261, #9760, #16435, #5363, #13817, #6446, #8450, #9422, #2881, #15679, #8005, #15567, #14361, #9305 ) ) ;
#5842 = DIRECTION ( 'NONE',  ( 0.000000000000000000, 0.000000000000000000, -1.000000000000000000 ) ) ;
#5843 = CARTESIAN_POINT ( 'NONE',  ( -4.000000000000000888, -26.11032815671481444, -13.00793304497391567 ) ) ;
#5844 = DIRECTION ( 'NONE',  ( -0.000000000000000000, -1.000000000000000000, -0.000000000000000000 ) ) ;
#5845 = PRESENTATION_STYLE_ASSIGNMENT (( #11869 ) ) ;
#5846 = VERTEX_POINT ( 'NONE', #2639 ) ;
#5847 = CIRCLE ( 'NONE', #16526, 2.149999999999995470 ) ;
#5848 = CARTESIAN_POINT ( 'NONE',  ( 1.027846397803612311, 21.25319992234354416, 3.346150245485499219 ) ) ;
#5849 = CARTESIAN_POINT ( 'NONE',  ( -1.071796769724486786, -23.14483002428746161, -15.74654998063472533 ) ) ;
#5850 = CARTESIAN_POINT ( 'NONE',  ( 4.243569643750000786, -22.19029169917569888, -7.409540791782929681 ) ) ;
#5851 = CARTESIAN_POINT ( 'NONE',  ( 2.798362969681366330, 38.99680007765647360, -2.102939460078824929 ) ) ;
#5852 = ADVANCED_FACE ( 'NONE', ( #18141 ), #6023, .T. ) ;
#5853 = CARTESIAN_POINT ( 'NONE',  ( 2.798362969681409851, 33.50319992234354771, 2.102939460078764977 ) ) ;
#5854 = CARTESIAN_POINT ( 'NONE',  ( -1.071796769724477238, -24.42985715469874108, -3.634184550572240546 ) ) ;
#5855 = DIRECTION ( 'NONE',  ( 0.000000000000000000, 0.000000000000000000, -1.000000000000000000 ) ) ;
#5856 = EDGE_CURVE ( 'NONE', #6787, #14266, #2277, .T. ) ;
#5857 = CARTESIAN_POINT ( 'NONE',  ( -2.121784821874996396, -19.90043129408965328, -10.54651638600367214 ) ) ;
#5858 = CARTESIAN_POINT ( 'NONE',  ( -7.144308362346979635, -13.70017171021367020, 0.6967212589853186699 ) ) ;
#5859 = VECTOR ( 'NONE', #871, 1000.000000000000000 ) ;
#5860 = AXIS2_PLACEMENT_3D ( 'NONE', #11510, #7340, #594 ) ;
#5861 = CARTESIAN_POINT ( 'NONE',  ( -8.500000000000010658, 10.00000000000000000, 20.49999999999998934 ) ) ;
#5862 = DIRECTION ( 'NONE',  ( -0.000000000000000000, 1.000000000000000000, -0.000000000000000000 ) ) ;
#5863 = CARTESIAN_POINT ( 'NONE',  ( -3.999999999999997335, -22.88501232838376254, -12.42802258070763877 ) ) ;
#5864 = CARTESIAN_POINT ( 'NONE',  ( 4.243569643750003451, -18.61318233583002879, -6.572389296263599689 ) ) ;
#5865 = CARTESIAN_POINT ( 'NONE',  ( -1.048844091575818815, 15.00000000000000888, -3.317259973752782809 ) ) ;
#5866 = DIRECTION ( 'NONE',  ( -0.000000000000000000, -1.000000000000000000, -0.000000000000000000 ) ) ;
#5867 = EDGE_LOOP ( 'NONE', ( #4127, #15925, #15176, #4420 ) ) ;
#5868 = CARTESIAN_POINT ( 'NONE',  ( 1.497042530366522461, 18.62819992234354771, 2.161531897785029965 ) ) ;
#5869 = CARTESIAN_POINT ( 'NONE',  ( 2.121784821875004390, -23.52471740128279620, -15.72253336585475658 ) ) ;
#5870 = CARTESIAN_POINT ( 'NONE',  ( -0.05938372350928957516, 18.62180007765647716, -4.731580009072201776 ) ) ;
#5871 = MECHANICAL_DESIGN_GEOMETRIC_PRESENTATION_REPRESENTATION (  '', ( #12384 ), #10906 ) ;
#5872 = DIRECTION ( 'NONE',  ( 1.000000000000000000, 0.000000000000000000, 0.000000000000000000 ) ) ;
#5873 = EDGE_CURVE ( 'NONE', #7574, #4547, #10769, .T. ) ;
#5874 = AXIS2_PLACEMENT_3D ( 'NONE', #13715, #6848, #5278 ) ;
#5875 = DIRECTION ( 'NONE',  ( 0.8191520442889951292, 0.4698463103929522156, -0.3289899283371602867 ) ) ;
#5876 = VERTEX_POINT ( 'NONE', #10783 ) ;
#5877 = CARTESIAN_POINT ( 'NONE',  ( 2.121784821875004390, -16.84613677052036351, -6.184531750164772745 ) ) ;
#5878 = CARTESIAN_POINT ( 'NONE',  ( 2.864755990943265829, 29.49680007765647716, 2.011557305968487697 ) ) ;
#5879 = CARTESIAN_POINT ( 'NONE',  ( -5.330712181944245322E-15, -30.43072080220681386, -10.63511296669387818 ) ) ;
#5880 = CARTESIAN_POINT ( 'NONE',  ( 4.243569643750000786, -25.54571385182929077, -12.20158025087355114 ) ) ;
#5881 = CYLINDRICAL_SURFACE ( 'NONE', #17690, 4.000000000000000000 ) ;
#5882 = CIRCLE ( 'NONE', #12700, 0.9999999999999991118 ) ;
#5883 = PLANE ( 'NONE',  #7689 ) ;
#5884 = CARTESIAN_POINT ( 'NONE',  ( 0.000000000000000000, 5.977523610840987267, 32.81826849749789687 ) ) ;
#5885 = CARTESIAN_POINT ( 'NONE',  ( -2.121784821874996396, -22.19115218676662238, -13.81800486288284624 ) ) ;
#5886 = CARTESIAN_POINT ( 'NONE',  ( 6.428571428571432378, -14.26578344203647752, -2.827263138854379410 ) ) ;
#5887 = CARTESIAN_POINT ( 'NONE',  ( 4.713407268011036227E-15, -17.22916635242506800, -8.376955330780271325 ) ) ;
#5888 = CARTESIAN_POINT ( 'NONE',  ( 1.989345975306426206, 23.99680007765648071, -1.515154207786343799 ) ) ;
#5889 = ORIENTED_EDGE ( 'NONE', *, *, #12881, .T. ) ;
#5890 = CARTESIAN_POINT ( 'NONE',  ( 2.798362969681366330, 23.99680007765647716, -2.102939460078824929 ) ) ;
#5891 = CARTESIAN_POINT ( 'NONE',  ( 4.243569643750000786, -27.09437022997710187, -14.41329077045383578 ) ) ;
#5892 = CARTESIAN_POINT ( 'NONE',  ( 8.499999999999992895, 17.19999999999999929, 20.49999999999999645 ) ) ;
#5893 = VECTOR ( 'NONE', #7828, 1000.000000000000000 ) ;
#5894 = CARTESIAN_POINT ( 'NONE',  ( 1.989345975306457071, 36.00319992234354771, 1.515154207786300500 ) ) ;
#5895 = ORIENTED_EDGE ( 'NONE', *, *, #13971, .T. ) ;
#5896 = CARTESIAN_POINT ( 'NONE',  ( 4.730628863548789710E-15, -19.95090606146734658, -12.75434688024559904 ) ) ;
#5897 = CONICAL_SURFACE ( 'NONE', #13903, 2.000000000000001776, 1.029744260000000189 ) ;
#5898 = CARTESIAN_POINT ( 'NONE',  ( -3.673772985318219053, 33.24680007765647360, -2.599342558260952174 ) ) ;
#5899 = EDGE_LOOP ( 'NONE', ( #16314, #6311, #10342, #2522, #8737 ) ) ;
#5900 = CARTESIAN_POINT ( 'NONE',  ( -9.000000000000001776, 25.39999999999999503, 2.499999999999998224 ) ) ;
#5901 = CARTESIAN_POINT ( 'NONE',  ( 2.000000000000004441, -19.93878920005454347, -10.23353884610596509 ) ) ;
#5902 = ADVANCED_FACE ( 'NONE', ( #5318 ), #1016, .T. ) ;
#5903 = CARTESIAN_POINT ( 'NONE',  ( -5.330712181944245322E-15, -29.39828321677494216, -9.160639286973687234 ) ) ;
#5904 = CARTESIAN_POINT ( 'NONE',  ( 4.299564228933482956E-15, -17.92964144805248594, -8.298488810700408891 ) ) ;
#5905 = DIRECTION ( 'NONE',  ( 1.000000000000000000, 0.000000000000000000, -0.000000000000000000 ) ) ;
#5906 = ADVANCED_FACE ( 'NONE', ( #9388 ), #975, .F. ) ;
#5907 = CARTESIAN_POINT ( 'NONE',  ( -1.071796769724477238, -23.84911101218836293, -2.804793104722865582 ) ) ;
#5908 = CARTESIAN_POINT ( 'NONE',  ( 4.730628863548789710E-15, -17.62792149424562638, -9.436781100875167638 ) ) ;
#5909 = VERTEX_POINT ( 'NONE', #17949 ) ;
#5910 = EDGE_CURVE ( 'NONE', #1761, #16507, #5221, .T. ) ;
#5911 = AXIS2_PLACEMENT_3D ( 'NONE', #14423, #14332, #3299 ) ;
#5912 = DIRECTION ( 'NONE',  ( 1.000000000000000000, 0.000000000000000000, 1.224646799147353207E-16 ) ) ;
#5913 = VERTEX_POINT ( 'NONE', #15156 ) ;
#5914 = ORIENTED_EDGE ( 'NONE', *, *, #15782, .T. ) ;
#5915 = CARTESIAN_POINT ( 'NONE',  ( 3.999999999999993339, 0.000000000000000000, -4.999999999999997335 ) ) ;
#5916 = DIRECTION ( 'NONE',  ( 0.7601375407242620952, 0.6497622020259954390, 0.000000000000000000 ) ) ;
#5917 = EDGE_CURVE ( 'NONE', #12929, #1500, #5738, .T. ) ;
#5918 = CARTESIAN_POINT ( 'NONE',  ( -0.05938372350918959958, 21.37819992234354416, 4.731580009072201776 ) ) ;
#5919 = CARTESIAN_POINT ( 'NONE',  ( -2.798362969681409851, 27.25319992234354771, -2.102939460078765421 ) ) ;
#5920 = CARTESIAN_POINT ( 'NONE',  ( 2.055738996568281518, 15.50319992234354949, -1.423772053676066518 ) ) ;
#5921 = VERTEX_POINT ( 'NONE', #6698 ) ;
#5922 = CARTESIAN_POINT ( 'NONE',  ( 4.499999999999999112, 35.75319992234354061, 0.05647727720528474687 ) ) ;
#5923 = CARTESIAN_POINT ( 'NONE',  ( -5.279047395330986450E-15, -27.44179011682903635, -6.856821975206893960 ) ) ;
#5924 = ORIENTED_EDGE ( 'NONE', *, *, #13749, .T. ) ;
#5925 = EDGE_CURVE ( 'NONE', #4535, #2915, #8816, .T. ) ;
#5926 = AXIS2_PLACEMENT_3D ( 'NONE', #17300, #5862, #5951 ) ;
#5927 = CARTESIAN_POINT ( 'NONE',  ( 0.000000000000000000, 13.00000000000000178, 0.000000000000000000 ) ) ;
#5928 = CARTESIAN_POINT ( 'NONE',  ( 2.864755990943265829, 29.49680007765647716, 2.011557305968487697 ) ) ;
#5929 = CARTESIAN_POINT ( 'NONE',  ( -7.036060484405130211, -13.81968884013468291, -0.02068784084667009762 ) ) ;
#5930 = CARTESIAN_POINT ( 'NONE',  ( -2.121784821874996396, -18.31951124139709464, -8.288728563932130200 ) ) ;
#5931 = CARTESIAN_POINT ( 'NONE',  ( 2.829195390882805583, 29.62180007765647005, 3.793023760679204770 ) ) ;
#5932 = DIRECTION ( 'NONE',  ( 0.000000000000000000, 0.000000000000000000, 1.000000000000000000 ) ) ;
#5933 = ORIENTED_EDGE ( 'NONE', *, *, #4076, .T. ) ;
#5934 = ORIENTED_EDGE ( 'NONE', *, *, #10855, .T. ) ;
#5935 = CARTESIAN_POINT ( 'NONE',  ( 2.211161402132902243, 24.62180007765647716, 2.942372952327172442 ) ) ;
#5936 = DIRECTION ( 'NONE',  ( 0.000000000000000000, 0.000000000000000000, -1.000000000000000000 ) ) ;
#5937 = CARTESIAN_POINT ( 'NONE',  ( -3.999999999999997335, -24.69177810288954333, -15.00835152021797114 ) ) ;
#5938 = ORIENTED_EDGE ( 'NONE', *, *, #5024, .T. ) ;
#5939 = AXIS2_PLACEMENT_3D ( 'NONE', #16106, #11534, #10331 ) ;
#5940 = CARTESIAN_POINT ( 'NONE',  ( 1.135272562821020070, 20.25319992234354416, -3.311245368580577164 ) ) ;
#5941 = CARTESIAN_POINT ( 'NONE',  ( 0.000000000000000000, -27.20729309053124112, -14.57456132866985499 ) ) ;
#5942 = CARTESIAN_POINT ( 'NONE',  ( -2.121784821875005722, -25.80296276059631921, -6.161734599703687643 ) ) ;
#5943 = CARTESIAN_POINT ( 'NONE',  ( -2.864755990943265829, 38.24680007765647360, -2.011557305968488141 ) ) ;
#5944 = APPLICATION_CONTEXT ( 'automotive_design' ) ;
#5945 = CARTESIAN_POINT ( 'NONE',  ( -1.135272562821019626, 36.50319992234354061, 3.311245368580577164 ) ) ;
#5946 = CARTESIAN_POINT ( 'NONE',  ( 1.071796769724495224, -16.45703912041794936, -6.195394731765314411 ) ) ;
#5947 = CARTESIAN_POINT ( 'NONE',  ( -4.000000000000004441, -28.94847988909901915, -13.03491587733159385 ) ) ;
#5948 = CARTESIAN_POINT ( 'NONE',  ( -4.243569643749997233, -20.88239411214383523, -9.813159571481939736 ) ) ;
#5949 = CYLINDRICAL_SURFACE ( 'NONE', #9217, 4.000000000000000000 ) ;
#5950 = CARTESIAN_POINT ( 'NONE',  ( -5.562324373798915644, -10.00000000000000178, -9.830817939998720334 ) ) ;
#5951 = DIRECTION ( 'NONE',  ( 0.000000000000000000, 0.000000000000000000, 1.000000000000000000 ) ) ;
#5952 = ORIENTED_EDGE ( 'NONE', *, *, #17851, .T. ) ;
#5953 = CARTESIAN_POINT ( 'NONE',  ( -5.330712181944245322E-15, -25.23626920050269362, -3.216667265601666603 ) ) ;
#5954 = DIRECTION ( 'NONE',  ( -1.000000000000000000, -0.000000000000000000, -0.000000000000000000 ) ) ;
#5955 = FACE_OUTER_BOUND ( 'NONE', #2043, .T. ) ;
#5956 = EDGE_LOOP ( 'NONE', ( #17139, #13510, #439, #7516 ) ) ;
#5957 = CARTESIAN_POINT ( 'NONE',  ( -1.497042530366522461, 17.37819992234354416, -2.161531897785030409 ) ) ;
#5958 = FACE_OUTER_BOUND ( 'NONE', #16146, .T. ) ;
#5959 = DIRECTION ( 'NONE',  ( -0.000000000000000000, -1.000000000000000000, -0.000000000000000000 ) ) ;
#5960 = CARTESIAN_POINT ( 'NONE',  ( -2.733110507866247652, 17.62180007765648071, 3.862833514489154574 ) ) ;
#5961 = CARTESIAN_POINT ( 'NONE',  ( 0.000000000000000000, 0.000000000000000000, -30.00000000000000000 ) ) ;
#5962 = CARTESIAN_POINT ( 'NONE',  ( 7.951672694476628500, -10.00000000000000178, -6.265341990737701927 ) ) ;
#5963 = ORIENTED_EDGE ( 'NONE', *, *, #12523, .F. ) ;
#5964 = CARTESIAN_POINT ( 'NONE',  ( -0.05938372350927861171, 38.62180007765648071, -3.680117784833935701 ) ) ;
#5965 = CARTESIAN_POINT ( 'NONE',  ( 4.243569643750003451, -24.32385273025008843, -14.72807183721590718 ) ) ;
#5966 = AXIS2_PLACEMENT_3D ( 'NONE', #18198, #11109, #13717 ) ;
#5967 = ADVANCED_FACE ( 'NONE', ( #16651 ), #12837, .T. ) ;
#5968 = CARTESIAN_POINT ( 'NONE',  ( 13.00000000000000178, 15.00000000000000178, -16.00000000000000000 ) ) ;
#5969 =( GEOMETRIC_REPRESENTATION_CONTEXT ( 3 ) GLOBAL_UNCERTAINTY_ASSIGNED_CONTEXT ( ( #6741 ) ) GLOBAL_UNIT_ASSIGNED_CONTEXT ( ( #3895, #8151, #15036 ) ) REPRESENTATION_CONTEXT ( 'NONE', 'WORKASPACE' ) );
#5970 = CARTESIAN_POINT ( 'NONE',  ( 2.121784821874994176, -28.85725728416562674, -10.52371923554258260 ) ) ;
#5971 = CARTESIAN_POINT ( 'NONE',  ( -11.99999999999999822, 48.00000000000000000, -15.00000000000000000 ) ) ;
#5972 = PRODUCT_DEFINITION_FORMATION_WITH_SPECIFIED_SOURCE ( 'ANY', '', #2369, .NOT_KNOWN. ) ;
#5973 = CARTESIAN_POINT ( 'NONE',  ( -1.071796769724496334, -21.33806424978168081, -13.16622104112438407 ) ) ;
#5974 = EDGE_CURVE ( 'NONE', #14789, #7076, #15789, .T. ) ;
#5975 = LINE ( 'NONE', #13118, #2023 ) ;
#5976 = CARTESIAN_POINT ( 'NONE',  ( 4.243569643750000786, -24.51327626639741553, -10.72710657115335842 ) ) ;
#5977 = FACE_OUTER_BOUND ( 'NONE', #16084, .T. ) ;
#5978 = CARTESIAN_POINT ( 'NONE',  ( -4.000000000000000888, -20.94814022955544175, -5.635564646372960951 ) ) ;
#5979 = CARTESIAN_POINT ( 'NONE',  ( -2.055738996568313048, 20.74680007765648071, -1.423772053676023441 ) ) ;
#5980 = VERTEX_POINT ( 'NONE', #2903 ) ;
#5981 = CARTESIAN_POINT ( 'NONE',  ( -1.027846397803541700, 19.99680007765648071, 3.346150245485522312 ) ) ;
#5982 = DIRECTION ( 'NONE',  ( 0.000000000000000000, 0.000000000000000000, -1.000000000000000000 ) ) ;
#5983 = DIRECTION ( 'NONE',  ( 0.000000000000000000, 0.000000000000000000, 1.000000000000000000 ) ) ;
#5984 = AXIS2_PLACEMENT_3D ( 'NONE', #8875, #12613, #1234 ) ;
#5985 = DIRECTION ( 'NONE',  ( 0.000000000000000000, 0.000000000000000000, 1.000000000000000000 ) ) ;
#5986 = CARTESIAN_POINT ( 'NONE',  ( -3.518350579753605434, 19.37819992234354416, 1.080741659609877781 ) ) ;
#5987 = VERTEX_POINT ( 'NONE', #16834 ) ;
#5988 = CARTESIAN_POINT ( 'NONE',  ( -4.243569643750004339, -26.66002939159266916, -9.521497656227012385 ) ) ;
#5989 = CARTESIAN_POINT ( 'NONE',  ( -4.481649420246366589, 37.87180007765647360, 1.518615910253458878 ) ) ;
#5990 = ORIENTED_EDGE ( 'NONE', *, *, #17333, .T. ) ;
#5991 = SURFACE_STYLE_USAGE ( .BOTH. , #17708 ) ;
#5992 = CARTESIAN_POINT ( 'NONE',  ( 1.999999999999994449, -25.70007750483700448, -6.382557533612111200 ) ) ;
#5993 = CARTESIAN_POINT ( 'NONE',  ( -4.243569643750005227, -27.95057637338251411, -11.36458975587725106 ) ) ;
#5994 = CARTESIAN_POINT ( 'NONE',  ( 1.300000000000000044, -1.443375672974064328, 1.278502688459867223E-18 ) ) ;
#5995 = DIRECTION ( 'NONE',  ( -0.6427862986982413318, -0.6275077727036082464, 0.4393856727322503208 ) ) ;
#5996 = COLOUR_RGB ( '',0.8941176470588234615, 0.8941176470588234615, 0.8941176470588234615 ) ;
#5997 = CARTESIAN_POINT ( 'NONE',  ( 1.999999999999994449, -26.53893304370534523, -7.580567399391532568 ) ) ;
#5998 =( BOUNDED_CURVE ( )  B_SPLINE_CURVE ( 3, ( #12612, #6867, #8434, #13331 ),
 .UNSPECIFIED., .F., .T. ) 
 B_SPLINE_CURVE_WITH_KNOTS ( ( 4, 4 ),
 ( 4.712388980384689674, 6.283185307179585344 ),
 .UNSPECIFIED. ) 
 CURVE ( )  GEOMETRIC_REPRESENTATION_ITEM ( )  RATIONAL_B_SPLINE_CURVE ( ( 1.000000000000000000, 0.8047378541243649375, 0.8047378541243649375, 1.000000000000000000 ) ) 
 REPRESENTATION_ITEM ( '' )  );
#5999 = CARTESIAN_POINT ( 'NONE',  ( 2.121784821875004390, -18.39479314866817461, -8.396242269745057385 ) ) ;
#6000 = ORIENTED_EDGE ( 'NONE', *, *, #5135, .F. ) ;
#6001 = CARTESIAN_POINT ( 'NONE',  ( 1.071796769724476128, -18.97360573420318985, -9.789424325076520716 ) ) ;
#6002 = CARTESIAN_POINT ( 'NONE',  ( 8.000000000000000000, 36.39999999999999147, -2.500000000000000888 ) ) ;
#6003 = ORIENTED_EDGE ( 'NONE', *, *, #5062, .F. ) ;
#6004 = ORIENTED_EDGE ( 'NONE', *, *, #11127, .T. ) ;
#6005 = CARTESIAN_POINT ( 'NONE',  ( 13.00000000000000178, 13.00000000000000178, -25.00000000000000355 ) ) ;
#6006 = CARTESIAN_POINT ( 'NONE',  ( 8.500000000000001776, 10.00000000000000000, -22.64999999999999503 ) ) ;
#6007 = CARTESIAN_POINT ( 'NONE',  ( -4.481649420246396787, 24.62819992234354416, -1.518615910253363399 ) ) ;
#6008 = CARTESIAN_POINT ( 'NONE',  ( -3.500000000000000444, 24.50319992234354416, -0.05647727720529563400 ) ) ;
#6009 = CARTESIAN_POINT ( 'NONE',  ( 2.481649420246391902, 20.87819992234355126, 0.8687765177875720335 ) ) ;
#6010 = EDGE_CURVE ( 'NONE', #14506, #15334, #14986, .T. ) ;
#6011 = AXIS2_PLACEMENT_3D ( 'NONE', #10987, #15083, #899 ) ;
#6012 = VERTEX_POINT ( 'NONE', #5497 ) ;
#6013 = CARTESIAN_POINT ( 'NONE',  ( -3.673772985318163098, 31.75319992234354771, 2.599342558261029001 ) ) ;
#6014 = VECTOR ( 'NONE', #6757, 1000.000000000000000 ) ;
#6015 = CARTESIAN_POINT ( 'NONE',  ( -4.000000000000004441, -24.56062015101355556, -6.768402738520779671 ) ) ;
#6016 = ORIENTED_EDGE ( 'NONE', *, *, #12317, .F. ) ;
#6017 = EDGE_CURVE ( 'NONE', #6744, #3421, #4104, .T. ) ;
#6018 = CARTESIAN_POINT ( 'NONE',  ( -5.577813053751546416E-15, -24.16022105762192851, -3.249104295986281699 ) ) ;
#6019 = CARTESIAN_POINT ( 'NONE',  ( 1.027846397803542144, 26.24680007765648071, -3.346150245485522312 ) ) ;
#6020 = CARTESIAN_POINT ( 'NONE',  ( 1.071796769724494780, -27.18147976340427974, -7.563908894501662594 ) ) ;
#6021 = CARTESIAN_POINT ( 'NONE',  ( 4.730628863548789710E-15, -17.59565781970088238, -9.390703798383912115 ) ) ;
#6022 = CARTESIAN_POINT ( 'NONE',  ( 2.733110507866247652, 33.87180007765647360, -3.862833514489153686 ) ) ;
#6023 = TOROIDAL_SURFACE ( 'NONE', #14639, 9.000000000000001776, 0.9999999999999991118 ) ;
#6024 = FACE_OUTER_BOUND ( 'NONE', #11846, .T. ) ;
#6025 = ORIENTED_EDGE ( 'NONE', *, *, #2773, .T. ) ;
#6026 = CARTESIAN_POINT ( 'NONE',  ( -0.05938372350927861171, 31.12180007765647005, -3.680117784833935701 ) ) ;
#6027 = CARTESIAN_POINT ( 'NONE',  ( 0.000000000000000000, 38.59999999999999432, 2.500000000000000000 ) ) ;
#6028 = DIRECTION ( 'NONE',  ( 0.000000000000000000, 1.000000000000000000, -9.859324684083080328E-16 ) ) ;
#6029 = CARTESIAN_POINT ( 'NONE',  ( 0.000000000000000000, 5.977523610840987267, 32.81826849749789687 ) ) ;
#6030 = ORIENTED_EDGE ( 'NONE', *, *, #11119, .T. ) ;
#6031 = CARTESIAN_POINT ( 'NONE',  ( -2.115076519116425580, 27.37819992234354771, -3.012182706137062738 ) ) ;
#6032 = CARTESIAN_POINT ( 'NONE',  ( 4.000000000000000000, 3.518949890710770134, -4.119968255444916849E-15 ) ) ;
#6033 = CARTESIAN_POINT ( 'NONE',  ( 2.121784821874994176, -23.95317875336422020, -3.519969256871676055 ) ) ;
#6034 = CARTESIAN_POINT ( 'NONE',  ( 3.500000000000000444, 36.74680007765648071, -0.05647727720536935281 ) ) ;
#6035 = EDGE_CURVE ( 'NONE', #15989, #13645, #8698, .T. ) ;
#6036 = EDGE_CURVE ( 'NONE', #10707, #2844, #4286, .T. ) ;
#6037 = CARTESIAN_POINT ( 'NONE',  ( -3.500000000000000444, 34.50319992234354771, -0.05647727720529563400 ) ) ;
#6038 = CARTESIAN_POINT ( 'NONE',  ( 4.299564228933482956E-15, -16.44551241969911359, -6.178932897109397970 ) ) ;
#6039 = ADVANCED_FACE ( 'NONE', ( #14390 ), #4901, .T. ) ;
#6040 = CARTESIAN_POINT ( 'NONE',  ( 2.000000000000004441, -22.77799255999219952, -14.28834146533649196 ) ) ;
#6041 = CARTESIAN_POINT ( 'NONE',  ( -4.243569643750000786, -22.60971946825739209, -8.008545724169261248 ) ) ;
#6042 = DIRECTION ( 'NONE',  ( 0.000000000000000000, 1.000000000000000000, 0.000000000000000000 ) ) ;
#6043 = PRESENTATION_LAYER_ASSIGNMENT (  '', '', ( #1322 ) ) ;
#6044 = CARTESIAN_POINT ( 'NONE',  ( -5.463737038710864802, -14.68677294254779220, -5.668536799318995456 ) ) ;
#6045 = CARTESIAN_POINT ( 'NONE',  ( 4.000000000000000000, 0.000000000000000000, 0.000000000000000000 ) ) ;
#6046 = DIRECTION ( 'NONE',  ( -1.000000000000000000, 0.000000000000000000, 4.336808689942021680E-16 ) ) ;
#6047 = VERTEX_POINT ( 'NONE', #2733 ) ;
#6048 = ORIENTED_EDGE ( 'NONE', *, *, #11270, .T. ) ;
#6049 = LINE ( 'NONE', #6337, #6760 ) ;
#6050 = CARTESIAN_POINT ( 'NONE',  ( -10.00000000000000178, 31.99999999999999289, -2.500000000000001776 ) ) ;
#6051 = DIRECTION ( 'NONE',  ( 1.000000000000000000, 0.000000000000000000, 0.000000000000000000 ) ) ;
#6052 = VERTEX_POINT ( 'NONE', #1514 ) ;
#6053 = CARTESIAN_POINT ( 'NONE',  ( -2.500000000000001332, 17.00319992234354416, -0.05647727720530596601 ) ) ;
#6054 = CARTESIAN_POINT ( 'NONE',  ( -4.243569643750005227, -27.40209390612182716, -10.58127561352589829 ) ) ;
#6055 = CARTESIAN_POINT ( 'NONE',  ( 2.864755990943265829, 16.99680007765647716, 2.011557305968487697 ) ) ;
#6056 = DIRECTION ( 'NONE',  ( -1.000000000000000000, 0.000000000000000000, -0.000000000000000000 ) ) ;
#6057 = CARTESIAN_POINT ( 'NONE',  ( 5.463737038711272476, -14.68677294254804977, -5.668536799318668606 ) ) ;
#6058 = ORIENTED_EDGE ( 'NONE', *, *, #11239, .T. ) ;
#6059 = CARTESIAN_POINT ( 'NONE',  ( 2.211161402132902243, 37.12180007765645939, 2.942372952327172442 ) ) ;
#6060 = CARTESIAN_POINT ( 'NONE',  ( 2.121784821875004390, -23.55698107582754730, -15.76861066834601210 ) ) ;
#6061 = ADVANCED_FACE ( 'NONE', ( #10019 ), #8537, .F. ) ;
#6062 = CARTESIAN_POINT ( 'NONE',  ( -4.243569643750004339, -27.91831269883777011, -11.31851245338599732 ) ) ;
#6063 = FACE_OUTER_BOUND ( 'NONE', #3865, .T. ) ;
#6064 = DIRECTION ( 'NONE',  ( -3.469446951953613696E-16, -0.000000000000000000, -1.000000000000000000 ) ) ;
#6065 = CARTESIAN_POINT ( 'NONE',  ( 1.071796769724490339, -22.65166463300919730, -15.04223681008646096 ) ) ;
#6066 = CARTESIAN_POINT ( 'NONE',  ( -5.330712181944245322E-15, -29.36601954223019462, -9.114561984482429935 ) ) ;
#6067 = CARTESIAN_POINT ( 'NONE',  ( -8.000000000000000000, 43.00000000000000000, 2.500000000000000000 ) ) ;
#6068 = CARTESIAN_POINT ( 'NONE',  ( 3.999999999999996447, -22.73234526084956286, -4.157355598356369697 ) ) ;
#6069 = CARTESIAN_POINT ( 'NONE',  ( -0.05938372350926768989, 21.12180007765648426, -2.628655560595669183 ) ) ;
#6070 = EDGE_LOOP ( 'NONE', ( #11748, #14296, #12022, #9434 ) ) ;
#6071 = CARTESIAN_POINT ( 'NONE',  ( -2.115076519116362519, 20.12180007765647716, 3.012182706137108035 ) ) ;
#6072 = CARTESIAN_POINT ( 'NONE',  ( -2.000000000000005773, -26.58195127643166700, -7.642003802713210447 ) ) ;
#6073 = CARTESIAN_POINT ( 'NONE',  ( 0.000000000000000000, 0.000000000000000000, 0.000000000000000000 ) ) ;
#6074 = CARTESIAN_POINT ( 'NONE',  ( 4.000000000000000888, -26.49749225125177432, -13.56086067486898372 ) ) ;
#6075 = CARTESIAN_POINT ( 'NONE',  ( 0.000000000000000000, 33.00000000000000000, 0.000000000000000000 ) ) ;
#6076 = CARTESIAN_POINT ( 'NONE',  ( 0.05938372350920109732, 22.62819992234354416, -3.680117784833935701 ) ) ;
#6077 = EDGE_CURVE ( 'NONE', #13336, #17808, #18317, .T. ) ;
#6078 = VERTEX_POINT ( 'NONE', #4198 ) ;
#6079 = CARTESIAN_POINT ( 'NONE',  ( -2.121784821875005722, -26.60955462421497586, -7.313667161985088150 ) ) ;
#6080 = CIRCLE ( 'NONE', #10226, 0.9999999999999991118 ) ;
#6081 = CARTESIAN_POINT ( 'NONE',  ( -2.211161402132902243, 18.37180007765647005, -2.942372952327172886 ) ) ;
#6082 = ORIENTED_EDGE ( 'NONE', *, *, #7843, .F. ) ;
#6083 = VECTOR ( 'NONE', #2923, 1000.000000000000000 ) ;
#6084 = ADVANCED_FACE ( 'NONE', ( #9846 ), #15863, .T. ) ;
#6085 = VECTOR ( 'NONE', #14166, 1000.000000000000000 ) ;
#6086 = CARTESIAN_POINT ( 'NONE',  ( -1.999999999999996225, -19.70218892076468364, -9.895638628843521190 ) ) ;
#6087 = CARTESIAN_POINT ( 'NONE',  ( 4.243569643749996345, -27.86453990792986701, -11.24171694923389531 ) ) ;
#6088 = CARTESIAN_POINT ( 'NONE',  ( -3.999999999999997335, -23.46575847089413713, -13.25741402655701506 ) ) ;
#6089 = CARTESIAN_POINT ( 'NONE',  ( 9.184850993605147944E-16, -10.54254386713301628, 22.30101802474215589 ) ) ;
#6090 = DIRECTION ( 'NONE',  ( -0.000000000000000000, -1.000000000000000000, -0.000000000000000000 ) ) ;
#6091 = CARTESIAN_POINT ( 'NONE',  ( -4.243569643750000786, -21.57728188282551685, -6.534072044449069416 ) ) ;
#6092 = ORIENTED_EDGE ( 'NONE', *, *, #2099, .T. ) ;
#6093 = CARTESIAN_POINT ( 'NONE',  ( -1.071796769724505882, -16.69209511533825463, -6.531089482383521272 ) ) ;
#6094 = LINE ( 'NONE', #12705, #12804 ) ;
#6095 = CARTESIAN_POINT ( 'NONE',  ( 1.071796769724476128, -19.74793392327709540, -10.89527958486666392 ) ) ;
#6096 = ORIENTED_EDGE ( 'NONE', *, *, #3500, .F. ) ;
#6097 = ORIENTED_EDGE ( 'NONE', *, *, #14830, .F. ) ;
#6098 = AXIS2_PLACEMENT_3D ( 'NONE', #6970, #1064, #4105 ) ;
#6099 = CARTESIAN_POINT ( 'NONE',  ( -15.00000000000000178, 10.00000000000000000, 24.99999999999999645 ) ) ;
#6100 = FACE_OUTER_BOUND ( 'NONE', #16876, .T. ) ;
#6101 = CARTESIAN_POINT ( 'NONE',  ( -1.336863392178569088, 22.50319992234354416, -4.297206761780648421 ) ) ;
#6102 = CARTESIAN_POINT ( 'NONE',  ( 1.135272562821020070, 25.25319992234354416, -3.311245368580577164 ) ) ;
#6103 = CIRCLE ( 'NONE', #16486, 2.200000000000000622 ) ;
#6104 = CARTESIAN_POINT ( 'NONE',  ( 2.481649420246391902, 18.37819992234354416, 0.8687765177875720335 ) ) ;
#6105 = EDGE_LOOP ( 'NONE', ( #13504, #17153, #806, #7661 ) ) ;
#6106 = CARTESIAN_POINT ( 'NONE',  ( -4.518350579753632523, 18.12180007765647716, -1.405661355842698468 ) ) ;
#6107 = EDGE_CURVE ( 'NONE', #3217, #9347, #15521, .T. ) ;
#6108 = CARTESIAN_POINT ( 'NONE',  ( -4.000000000000004441, -24.30251075465558586, -6.399784318590734600 ) ) ;
#6109 = ORIENTED_EDGE ( 'NONE', *, *, #12288, .T. ) ;
#6110 = DIRECTION ( 'NONE',  ( 3.469446951953612217E-16, -0.000000000000000000, 1.000000000000000000 ) ) ;
#6111 = CARTESIAN_POINT ( 'NONE',  ( 3.500000000000000444, 26.74680007765648071, -0.05647727720536935281 ) ) ;
#6112 =( BOUNDED_CURVE ( )  B_SPLINE_CURVE ( 2, ( #1542, #5973, #15910, #1630, #3208, #7177, #12838, #17412, #8845 ),
 .UNSPECIFIED., .F., .F. ) 
 B_SPLINE_CURVE_WITH_KNOTS ( ( 3, 2, 2, 2, 3 ),
 ( 0.3189655172413793371, 0.3218390804597701105, 0.3275862068965517127, 0.3333333333333333148, 0.3362068965517241437 ),
 .UNSPECIFIED. ) 
 CURVE ( )  GEOMETRIC_REPRESENTATION_ITEM ( )  RATIONAL_B_SPLINE_CURVE ( ( 0.9330127018922194093, 0.9330127018922200755, 1.000000000000000000, 0.8660254037844387076, 1.000000000000000000, 0.8660254037844387076, 1.000000000000000000, 0.9330127018922187432, 0.9330127018922194093 ) ) 
 REPRESENTATION_ITEM ( '' )  );
#6113 = DIRECTION ( 'NONE',  ( 0.000000000000000000, -0.000000000000000000, 1.000000000000000000 ) ) ;
#6114 = CARTESIAN_POINT ( 'NONE',  ( 4.730628863548789710E-15, -17.07943902698494298, -8.653466958523816643 ) ) ;
#6115 = AXIS2_PLACEMENT_3D ( 'NONE', #8822, #10113, #15797 ) ;
#6116 = CARTESIAN_POINT ( 'NONE',  ( -3.673772985318219053, 28.24680007765647360, -2.599342558260952174 ) ) ;
#6117 = LINE ( 'NONE', #10281, #2053 ) ;
#6118 = ORIENTED_EDGE ( 'NONE', *, *, #1607, .F. ) ;
#6119 = CARTESIAN_POINT ( 'NONE',  ( -3.518350579753630747, 28.12180007765647360, -1.080741659609802729 ) ) ;
#6120 = CARTESIAN_POINT ( 'NONE',  ( 9.000000000000005329, -10.00000000000000178, 15.14468620625654083 ) ) ;
#6121 = FACE_OUTER_BOUND ( 'NONE', #6861, .T. ) ;
#6122 = CARTESIAN_POINT ( 'NONE',  ( 8.673617379884035472E-16, 1.899999999999999689, 0.000000000000000000 ) ) ;
#6123 = CARTESIAN_POINT ( 'NONE',  ( -2.000000000000005773, -29.35662728657488429, -11.60465181595445650 ) ) ;
#6124 = ORIENTED_EDGE ( 'NONE', *, *, #4555, .F. ) ;
#6125 = CARTESIAN_POINT ( 'NONE',  ( 2.211161402132839626, 30.37819992234354416, -2.942372952327218183 ) ) ;
#6126 = CARTESIAN_POINT ( 'NONE',  ( 4.299564228933482956E-15, -20.83337215778458074, -12.44544603592020771 ) ) ;
#6127 = CARTESIAN_POINT ( 'NONE',  ( 2.121784821875004390, -19.13685766319732906, -9.456020227043945070 ) ) ;
#6128 = CARTESIAN_POINT ( 'NONE',  ( -1.497042530366477164, 20.12180007765648071, 2.161531897785062384 ) ) ;
#6129 = CARTESIAN_POINT ( 'NONE',  ( 1.444289557195957086, 17.75319992234354061, -4.262301884875733471 ) ) ;
#6130 = CARTESIAN_POINT ( 'NONE',  ( 4.730628863548789710E-15, -22.53200002504703292, -16.44053107954607640 ) ) ;
#6131 = AXIS2_PLACEMENT_3D ( 'NONE', #17103, #2998, #17483 ) ;
#6132 = CARTESIAN_POINT ( 'NONE',  ( -2.000000000000005773, -29.09851789021691815, -11.23603339602441054 ) ) ;
#6133 = CARTESIAN_POINT ( 'NONE',  ( 4.730628863548789710E-15, -17.62792149424562638, -9.436781100875167638 ) ) ;
#6134 = LINE ( 'NONE', #7429, #8608 ) ;
#6135 = CARTESIAN_POINT ( 'NONE',  ( -0.6850780354679466555, -10.00000000000000355, -5.037014450716167602 ) ) ;
#6136 = ADVANCED_FACE ( 'NONE', ( #7147 ), #7238, .F. ) ;
#6137 = CARTESIAN_POINT ( 'NONE',  ( 0.000000000000000000, 5.977523610840987267, 32.81826849749789687 ) ) ;
#6138 = VECTOR ( 'NONE', #16977, 1000.000000000000000 ) ;
#6139 = ADVANCED_FACE ( 'NONE', ( #203 ), #12895, .T. ) ;
#6140 = CARTESIAN_POINT ( 'NONE',  ( 9.000000000000001776, 25.39999999999999503, -2.500000000000002665 ) ) ;
#6141 = ORIENTED_EDGE ( 'NONE', *, *, #6657, .T. ) ;
#6142 = AXIS2_PLACEMENT_3D ( 'NONE', #17845, #5111, #17935 ) ;
#6143 = ORIENTED_EDGE ( 'NONE', *, *, #8299, .T. ) ;
#6144 = CARTESIAN_POINT ( 'NONE',  ( 4.243569643750003451, -17.83885414675612324, -5.466534036473456482 ) ) ;
#6145 = DIRECTION ( 'NONE',  ( -0.000000000000000000, -0.5735764363510414965, -0.8191520442889950182 ) ) ;
#6146 = CARTESIAN_POINT ( 'NONE',  ( 0.000000000000000000, 13.00000000000000178, 0.000000000000000000 ) ) ;
#6147 = EDGE_CURVE ( 'NONE', #10707, #9790, #7523, .T. ) ;
#6148 = ORIENTED_EDGE ( 'NONE', *, *, #4955, .F. ) ;
#6149 = CARTESIAN_POINT ( 'NONE',  ( 0.8262555684460829442, 30.25319992234354771, -2.360188852285421302 ) ) ;
#6150 = CARTESIAN_POINT ( 'NONE',  ( 4.243569643749996345, -27.57416683702714622, -10.82702122681259205 ) ) ;
#6151 = CARTESIAN_POINT ( 'NONE',  ( -2.864755990943265829, 20.74680007765647716, -2.011557305968488141 ) ) ;
#6152 = EDGE_CURVE ( 'NONE', #8381, #1806, #3141, .T. ) ;
#6153 = DIRECTION ( 'NONE',  ( 0.000000000000000000, 0.000000000000000000, 1.000000000000000000 ) ) ;
#6154 = CARTESIAN_POINT ( 'NONE',  ( 4.898587196589413815E-16, 2.700915433685006750, 35.11257424290206330 ) ) ;
#6155 = VERTEX_POINT ( 'NONE', #17476 ) ;
#6156 = CARTESIAN_POINT ( 'NONE',  ( 3.481649420246369697, 36.62180007765648071, -1.193696214020541824 ) ) ;
#6157 = COLOUR_RGB ( '',0.8941176470588234615, 0.8941176470588234615, 0.8941176470588234615 ) ;
#6158 = CARTESIAN_POINT ( 'NONE',  ( -2.121784821874996396, -23.25585344674324162, -15.33855584509429271 ) ) ;
#6159 = EDGE_CURVE ( 'NONE', #9378, #6179, #12990, .T. ) ;
#6160 = SURFACE_SIDE_STYLE ('',( #515 ) ) ;
#6161 = CARTESIAN_POINT ( 'NONE',  ( -5.330712181944246111E-15, -27.81736316408238352, -6.902851464902141743 ) ) ;
#6162 = CARTESIAN_POINT ( 'NONE',  ( 7.347880794884120722E-16, 33.00000000000000000, -6.000000000000000888 ) ) ;
#6163 = AXIS2_PLACEMENT_3D ( 'NONE', #3858, #1087, #9505 ) ;
#6164 = CARTESIAN_POINT ( 'NONE',  ( 4.299564228933482956E-15, -16.96173121241504944, -6.916169736969493442 ) ) ;
#6165 = CARTESIAN_POINT ( 'NONE',  ( -1.734723475976807094E-15, 18.79999999999999361, -2.500000000000000000 ) ) ;
#6166 = CARTESIAN_POINT ( 'NONE',  ( 4.243569643749996345, -24.73496347708949017, -6.772218607582066952 ) ) ;
#6167 = DIRECTION ( 'NONE',  ( 1.000000000000000000, 0.000000000000000000, 0.000000000000000000 ) ) ;
#6168 = FACE_OUTER_BOUND ( 'NONE', #8850, .T. ) ;
#6169 = COLOUR_RGB ( '',0.8941176470588234615, 0.8941176470588234615, 0.8941176470588234615 ) ;
#6170 = CARTESIAN_POINT ( 'NONE',  ( 2.500000000000001332, 34.24680007765648071, -0.05647727720535888202 ) ) ;
#6171 = CIRCLE ( 'NONE', #15954, 0.4999999999999992784 ) ;
#6172 = ORIENTED_EDGE ( 'NONE', *, *, #15787, .T. ) ;
#6173 = CARTESIAN_POINT ( 'NONE',  ( -2.864755990943265829, 23.24680007765647716, -2.011557305968488141 ) ) ;
#6174 = FACE_OUTER_BOUND ( 'NONE', #110, .T. ) ;
#6175 = DIRECTION ( 'NONE',  ( 0.000000000000000000, 0.000000000000000000, 1.000000000000000000 ) ) ;
#6176 = CARTESIAN_POINT ( 'NONE',  ( -3.999999999999997335, -23.46575847089413713, -13.25741402655701151 ) ) ;
#6177 = CARTESIAN_POINT ( 'NONE',  ( 4.299564228933482956E-15, -16.96173121241504944, -6.916169736969493442 ) ) ;
#6178 = CARTESIAN_POINT ( 'NONE',  ( -1.027846397803611866, 15.00319992234354594, -3.346150245485499219 ) ) ;
#6179 = VERTEX_POINT ( 'NONE', #15978 ) ;
#6180 = CARTESIAN_POINT ( 'NONE',  ( -2.121784821875005722, -26.09333583149904001, -6.576430322124992678 ) ) ;
#6181 = CARTESIAN_POINT ( 'NONE',  ( 3.481649420246369697, 19.12180007765648071, -1.193696214020541824 ) ) ;
#6182 = EDGE_LOOP ( 'NONE', ( #3265, #18000, #13060, #2389 ) ) ;
#6183 = AXIS2_PLACEMENT_3D ( 'NONE', #6371, #12015, #2032 ) ;
#6184 = CARTESIAN_POINT ( 'NONE',  ( 4.000000000000000888, -21.52888637065593258, -6.464956090208799466 ) ) ;
#6185 = CARTESIAN_POINT ( 'NONE',  ( -9.000000000000003553, 38.59999999999999432, -2.500000000000001776 ) ) ;
#6186 = CARTESIAN_POINT ( 'NONE',  ( -5.330712181944245322E-15, -29.91450200949088156, -9.897876126833780930 ) ) ;
#6187 = LINE ( 'NONE', #13226, #12611 ) ;
#6188 = PLANE ( 'NONE',  #13605 ) ;
#6189 = CARTESIAN_POINT ( 'NONE',  ( 1.533898589781675205E-14, -28.22544404955499786, -9.054844408877768203 ) ) ;
#6190 = CARTESIAN_POINT ( 'NONE',  ( -2.121784821875005722, -23.25413247156138397, -2.521627702894468470 ) ) ;
#6191 = ORIENTED_EDGE ( 'NONE', *, *, #14860, .T. ) ;
#6192 = CARTESIAN_POINT ( 'NONE',  ( -1.071796769724486564, -26.75284172192045062, -6.951750329942670170 ) ) ;
#6193 = CARTESIAN_POINT ( 'NONE',  ( 2.000000000000004441, -20.00331654984898577, -10.32569345209524414 ) ) ;
#6194 = DIRECTION ( 'NONE',  ( -0.000000000000000000, -1.000000000000000000, -0.000000000000000000 ) ) ;
#6195 = EDGE_LOOP ( 'NONE', ( #6096, #3063, #6109, #16703 ) ) ;
#6196 = ORIENTED_EDGE ( 'NONE', *, *, #2416, .T. ) ;
#6197 = CARTESIAN_POINT ( 'NONE',  ( -1.071796769724477238, -24.62343920126227559, -3.910648364513010122 ) ) ;
#6198 = DIRECTION ( 'NONE',  ( -0.000000000000000000, -1.000000000000000000, -0.000000000000000000 ) ) ;
#6199 = VECTOR ( 'NONE', #6909, 1000.000000000000000 ) ;
#6200 = CARTESIAN_POINT ( 'NONE',  ( -0.05938372350918959958, 23.87819992234354416, 4.731580009072201776 ) ) ;
#6201 = CARTESIAN_POINT ( 'NONE',  ( 3.500000000000000444, 38.25319992234354061, 0.05647727720529520379 ) ) ;
#6202 = VECTOR ( 'NONE', #928, 1000.000000000000000 ) ;
#6203 = CARTESIAN_POINT ( 'NONE',  ( 0.05938372350921204690, 20.12819992234354771, -2.628655560595669183 ) ) ;
#6204 = EDGE_LOOP ( 'NONE', ( #6356, #2272 ) ) ;
#6205 = CARTESIAN_POINT ( 'NONE',  ( -2.829195390882805139, 18.37180007765647360, -3.793023760679206102 ) ) ;
#6206 = CARTESIAN_POINT ( 'NONE',  ( -1.999999999999996225, -19.89577096732821104, -10.17210244278429343 ) ) ;
#6207 = EDGE_LOOP ( 'NONE', ( #498, #4275, #11171, #12765 ) ) ;
#6208 = CARTESIAN_POINT ( 'NONE',  ( -1.734723475976807094E-15, 36.39999999999999147, -2.500000000000000000 ) ) ;
#6209 = VECTOR ( 'NONE', #11246, 1000.000000000000000 ) ;
#6210 = CARTESIAN_POINT ( 'NONE',  ( 3.500000000000000444, 31.74680007765647716, -0.05647727720536935281 ) ) ;
#6211 = CARTESIAN_POINT ( 'NONE',  ( 0.000000000000000000, 25.39999999999999503, 2.500000000000000000 ) ) ;
#6212 = AXIS2_PLACEMENT_3D ( 'NONE', #6625, #12546, #8097 ) ;
#6213 = CARTESIAN_POINT ( 'NONE',  ( 2.121784821874994176, -24.46939754608015605, -4.257206096731771083 ) ) ;
#6214 = CARTESIAN_POINT ( 'NONE',  ( -2.121784821875005722, -27.64199220964684756, -8.788140841705278206 ) ) ;
#6215 = FACE_OUTER_BOUND ( 'NONE', #13517, .T. ) ;
#6216 = EDGE_CURVE ( 'NONE', #6155, #18310, #6231, .T. ) ;
#6217 = ORIENTED_EDGE ( 'NONE', *, *, #15676, .F. ) ;
#6218 = CARTESIAN_POINT ( 'NONE',  ( -0.9009846993709869079, -10.00000000000000178, 24.02174733379527538 ) ) ;
#6219 = DIRECTION ( 'NONE',  ( -1.000000000000000000, -0.000000000000000000, -0.000000000000000000 ) ) ;
#6220 = CARTESIAN_POINT ( 'NONE',  ( 0.000000000000000000, 5.000000000000000000, 0.000000000000000000 ) ) ;
#6221 = SURFACE_STYLE_FILL_AREA ( #195 ) ;
#6222 = ORIENTED_EDGE ( 'NONE', *, *, #5017, .T. ) ;
#6223 = CARTESIAN_POINT ( 'NONE',  ( -1.135272562821019626, 26.50319992234354771, 3.311245368580577164 ) ) ;
#6224 = DIRECTION ( 'NONE',  ( -4.915049848600951133E-16, 0.000000000000000000, -1.000000000000000000 ) ) ;
#6225 = CARTESIAN_POINT ( 'NONE',  ( 4.730628863548789710E-15, -17.07943902698494298, -8.653466958523816643 ) ) ;
#6226 = CARTESIAN_POINT ( 'NONE',  ( 1.593127413382998903, 24.62180007765647716, 2.091722143975139669 ) ) ;
#6227 = VECTOR ( 'NONE', #8823, 1000.000000000000000 ) ;
#6228 = CARTESIAN_POINT ( 'NONE',  ( 0.05938372350919016857, 17.62819992234354416, -4.731580009072201776 ) ) ;
#6229 = CARTESIAN_POINT ( 'NONE',  ( 4.243569643750000786, -26.35230571544794387, -13.35351281315494987 ) ) ;
#6230 = CARTESIAN_POINT ( 'NONE',  ( -3.999999999999997335, -24.43366870653157363, -14.63973310028792696 ) ) ;
#6231 =( BOUNDED_CURVE ( )  B_SPLINE_CURVE ( 2, ( #11596, #14588, #17572, #10395, #17292, #11689, #679, #14495, #10200, #15879, #3176, #488, #16255, #2075, #4927, #8814, #17380, #14778, #4645, #14687, #16073, #1793, #10298, #3274, #8911, #1891, #13176, #6130, #1695, #3367, #13365, #1983, #10579, #13270, #7705, #587, #6229, #4841, #10490, #11973, #17665, #3547, #9192, #2594, #5449, #8227, #6924, #5633, #1377, #7799, #2169, #13890, #5268, #13456, #16602, #9619, #9526, #7006, #12306, #12669, #14873, #768, #2686, #6413, #4151, #18359, #17997, #13797, #1201, #11096, #6837, #12579, #11275, #16964, #10923, #3878, #12487, #15206, #2507, #8135, #15293, #16689, #16782, #1105, #5362, #4243, #4051, #18180, #16873, #9703, #15387, #8318, #13979, #14063, #6745, #12400, #1292, #18092, #18267, #11009, #5537, #11184, #3968, #9798, #15479, #2776, #8406, #8486, #5722, #4417, #11362, #15558, #13130, #8668, #12939, #5988, #10060, #11546, #17052, #1469, #14158, #7472, #15737, #15645, #157, #12850, #3128, #5807, #11640, #1644, #251, #3039, #10247, #14345, #11450, #11731, #9886, #2853, #440, #1743, #2945, #8860, #7281, #14440, #7374, #10154, #17427, #5896, #14539, #4324, #7101, #17237, #13035, #4511, #12763, #8580, #1835, #9969, #67, #14253, #1555, #7193, #17140, #15832, #6079, #8763, #4597, #350, #17335, #15926, #3224, #7561, #3314, #16023, #3409, #17526, #10343, #11830, #4693, #1938, #16390, #7929, #17797, #901, #8957, #16204, #13218, #14635, #6180, #17619, #4788, #14998, #534, #2296, #6270, #3678, #3496, #10441, #6542, #9143, #10623, #13585, #12101, #12194, #16117, #7651, #9051, #14727, #6454, #13409, #14821, #2027, #3585, #5059, #720, #13317, #632, #11923, #4879, #10530, #2120, #6367, #7749, #12008, #9235, #17704, #4968, #16297, #14920, #10713, #2212, #7839, #13492, #807, #9324, #11076, #13771, #13956, #9597, #8204, #18066, #9777, #12561, #4129, #15455, #16668, #9680, #17973, #15365, #9502, #16851, #3947, #4033, #2663, #18159, #1354, #5338, #2752, #12284, #16480, #12375, #1084, #8382, #5151, #6903, #8022, #14045, #15273, #10808, #2572, #2390, #15085, #13675, #6985, #12465, #18246, #8297, #6637, #5515, #16760, #996, #1268, #10990, #6815, #15178, #3761, #11160, #17881, #13868, #9410, #5242, #10899, #16576, #3854, #1174, #2482, #5430, #8112, #6721, #3108, #11254, #13014, #133, #15538, #326, #8556, #46, #12830, #5785, #7077, #4303, #17034, #8647, #9950, #228, #11427, #17117, #14231, #4488, #7170, #15622, #8738, #1535, #1622, #1447, #7256, #5700, #14413, #4397, #14325, #12916, #15713, #12646, #10037, #1718, #12744, #16943, #3014, #5877, #11524, #5609, #17215, #2836, #7354, #10130, #4218, #15811, #8465, #9864 ),
 .UNSPECIFIED., .F., .T. ) 
 B_SPLINE_CURVE_WITH_KNOTS ( ( 3, 2, 2, 2, 2, 2, 2, 2, 2, 2, 2, 2, 2, 2, 2, 2, 2, 2, 2, 2, 2, 2, 2, 2, 2, 2, 2, 2, 2, 2, 2, 2, 2, 2, 2, 2, 2, 2, 2, 2, 2, 2, 2, 2, 2, 2, 2, 2, 2, 2, 2, 2, 2, 2, 2, 2, 2, 2, 2, 2, 2, 2, 2, 2, 2, 2, 2, 2, 2, 2, 2, 2, 2, 2, 2, 2, 2, 2, 2, 2, 2, 2, 2, 2, 2, 2, 2, 2, 2, 2, 2, 2, 2, 2, 2, 2, 2, 2, 2, 2, 2, 2, 2, 2, 2, 2, 2, 2, 2, 2, 2, 2, 2, 2, 2, 2, 2, 2, 2, 2, 2, 2, 2, 2, 2, 2, 2, 2, 2, 2, 2, 2, 2, 2, 2, 2, 2, 2, 2, 2, 2, 2, 2, 2, 2, 2, 2, 2, 2, 2, 2, 2, 2, 2, 2, 2, 2, 2, 2, 2, 2, 2, 2, 2, 2, 2, 2, 2, 2, 2, 2, 2, 2, 2, 3 ),
 ( 0.000000000000000000, 0.005769117196331985213, 0.01153823439266397043, 0.01730735158899595477, 0.02307646878532794085, 0.02884558598165992693, 0.03461470317799190954, 0.04038382037432389909, 0.04615293757065588170, 0.05192205476698786432, 0.05769117196331985387, 0.06346028915965185035, 0.06922940635598381909, 0.07499852355231581558, 0.08076764074864779819, 0.08653675794497978080, 0.09230587514131176341, 0.09807499233764375990, 0.1038441095339757286, 0.1096132267303077251, 0.1153823439266397077, 0.1211514611229717042, 0.1269205783193037007, 0.1326896955156356694, 0.1384588127119676382, 0.1442279299082996347, 0.1499970471046316312, 0.1557661643009635999, 0.1615352814972955964, 0.1673043986936275651, 0.1730735158899595616, 0.1788426330862915581, 0.1846117502826235268, 0.1903808674789554956, 0.1961499846752875198, 0.2019191018716194885, 0.2076882190679514573, 0.2134573362642834538, 0.2192264534606154502, 0.2249955706569474467, 0.2307646878532794155, 0.2365338050496113842, 0.2423029222459434084, 0.2480720394422753772, 0.2538411566386074014, 0.2596102738349393424, 0.2653793910312713389, 0.2711485082276033354, 0.2769176254239352764, 0.2826867426202672728, 0.2884558598165992693, 0.2942249770129312103, 0.2999940942092632623, 0.3057632114055952588, 0.3115323286019271998, 0.3173014457982591963, 0.3230705629945911928, 0.3288396801909231337, 0.3346087973872551302, 0.3403779145835871267, 0.3461470317799191232, 0.3519161489762511197, 0.3576852661725831162, 0.3634543833689150572, 0.3692235005652470536, 0.3749926177615790501, 0.3807617349579109911, 0.3865308521542429876, 0.3922999693505750396, 0.3980690865469069806, 0.4038382037432389771, 0.4096073209395709736, 0.4153764381359029145, 0.4211455553322349110, 0.4269146725285669075, 0.4326837897248988485, 0.4384529069212309005, 0.4442220241175628970, 0.4499911413138948935, 0.4557602585102268344, 0.4615293757065588309, 0.4672984929028908274, 0.4730676100992227684, 0.4788367272955547649, 0.4846058444918868169, 0.4903749616882187579, 0.4961440788845507543, 0.5019131960808826953, 0.5076823132772148028, 0.5134514304735466883, 0.5192205476698786848, 0.5249896648662106813, 0.5307587820625426778, 0.5365278992588745632, 0.5422970164552066707, 0.5480661336515386672, 0.5538352508478705527, 0.5596043680442026602, 0.5653734852405345457, 0.5711426024368665422, 0.5769117196331985387, 0.5826808368295305351, 0.5884499540258624206, 0.5942190712221945281, 0.5999881884185265246, 0.6057573056148584101, 0.6115264228111905176, 0.6172955400075224031, 0.6230646572038543995, 0.6288337744001863960, 0.6346028915965183925, 0.6403720087928503890, 0.6461411259891823855, 0.6519102431855143820, 0.6576793603818462675, 0.6634484775781783750, 0.6692175947745102604, 0.6749867119708422569, 0.6807558291671742534, 0.6865249463635062499, 0.6922940635598382464, 0.6980631807561702429, 0.7038322979525022394, 0.7096014151488341248, 0.7153705323451662323, 0.7211396495414981178, 0.7269087667378301143, 0.7326778839341622218, 0.7384470011304941073, 0.7442161183268261038, 0.7499852355231581003, 0.7557543527194900967, 0.7615234699158219822, 0.7672925871121540897, 0.7730617043084859752, 0.7788308215048179717, 0.7845999387011500792, 0.7903690558974819647, 0.7961381730938139611, 0.8019072902901459576, 0.8076764074864779541, 0.8134455246828098396, 0.8192146418791419471, 0.8249837590754739436, 0.8307528762718058291, 0.8365219934681379366, 0.8422911106644698220, 0.8480602278608018185, 0.8538293450571338150, 0.8595984622534658115, 0.8653675794497976970, 0.8711366966461298045, 0.8769058138424618010, 0.8826749310387936864, 0.8884440482351257939, 0.8942131654314576794, 0.8999822826277897869, 0.9057513998241216724, 0.9115205170204536689, 0.9172896342167857764, 0.9230587514131176619, 0.9288278686094496583, 0.9345969858057816548, 0.9403661030021136513, 0.9461352201984455368, 0.9519043373947776443, 0.9576734545911095298, 0.9634425717874415263, 0.9692116889837736338, 0.9749808061801055192, 0.9807499233764375157, 0.9865190405727695122, 0.9922881577691015087, 0.9980572749654333942, 1.000000000000000000 ),
 .UNSPECIFIED. ) 
 CURVE ( )  GEOMETRIC_REPRESENTATION_ITEM ( )  RATIONAL_B_SPLINE_CURVE ( ( 1.000000000000000000, 0.8660254037844387076, 1.000000000000000000, 0.8660254037844387076, 1.000000000000000000, 0.8660254037844387076, 1.000000000000000000, 0.8660254037844387076, 1.000000000000000000, 0.8660254037844387076, 1.000000000000000000, 0.8660254037844387076, 1.000000000000000000, 0.8660254037844387076, 1.000000000000000000, 0.8660254037844387076, 1.000000000000000000, 0.8660254037844387076, 1.000000000000000000, 0.8660254037844387076, 1.000000000000000000, 0.8660254037844387076, 1.000000000000000000, 0.8660254037844387076, 1.000000000000000000, 0.8660254037844387076, 1.000000000000000000, 0.8660254037844387076, 1.000000000000000000, 0.8660254037844387076, 1.000000000000000000, 0.8660254037844387076, 1.000000000000000000, 0.8660254037844387076, 1.000000000000000000, 0.8660254037844387076, 1.000000000000000000, 0.8660254037844387076, 1.000000000000000000, 0.8660254037844387076, 1.000000000000000000, 0.8660254037844387076, 1.000000000000000000, 0.8660254037844387076, 1.000000000000000000, 0.8660254037844387076, 1.000000000000000000, 0.8660254037844387076, 1.000000000000000000, 0.8660254037844387076, 1.000000000000000000, 0.8660254037844387076, 1.000000000000000000, 0.8660254037844387076, 1.000000000000000000, 0.8660254037844387076, 1.000000000000000000, 0.8660254037844387076, 1.000000000000000000, 0.8660254037844387076, 1.000000000000000000, 0.8660254037844387076, 1.000000000000000000, 0.8660254037844387076, 1.000000000000000000, 0.8660254037844387076, 1.000000000000000000, 0.8660254037844387076, 1.000000000000000000, 0.8660254037844387076, 1.000000000000000000, 0.8660254037844387076, 1.000000000000000000, 0.8660254037844387076, 1.000000000000000000, 0.8660254037844387076, 1.000000000000000000, 0.8660254037844387076, 1.000000000000000000, 0.8660254037844387076, 1.000000000000000000, 0.8660254037844387076, 1.000000000000000000, 0.8660254037844387076, 1.000000000000000000, 0.8660254037844387076, 1.000000000000000000, 0.8660254037844387076, 1.000000000000000000, 0.8660254037844387076, 1.000000000000000000, 0.8660254037844387076, 1.000000000000000000, 0.8660254037844387076, 1.000000000000000000, 0.8660254037844387076, 1.000000000000000000, 0.8660254037844387076, 1.000000000000000000, 0.8660254037844387076, 1.000000000000000000, 0.8660254037844387076, 1.000000000000000000, 0.8660254037844387076, 1.000000000000000000, 0.8660254037844387076, 1.000000000000000000, 0.8660254037844387076, 1.000000000000000000, 0.8660254037844387076, 1.000000000000000000, 0.8660254037844387076, 1.000000000000000000, 0.8660254037844387076, 1.000000000000000000, 0.8660254037844387076, 1.000000000000000000, 0.8660254037844387076, 1.000000000000000000, 0.8660254037844387076, 1.000000000000000000, 0.8660254037844387076, 1.000000000000000000, 0.8660254037844387076, 1.000000000000000000, 0.8660254037844387076, 1.000000000000000000, 0.8660254037844387076, 1.000000000000000000, 0.8660254037844387076, 1.000000000000000000, 0.8660254037844387076, 1.000000000000000000, 0.8660254037844387076, 1.000000000000000000, 0.8660254037844387076, 1.000000000000000000, 0.8660254037844387076, 1.000000000000000000, 0.8660254037844387076, 1.000000000000000000, 0.8660254037844387076, 1.000000000000000000, 0.8660254037844387076, 1.000000000000000000, 0.8660254037844387076, 1.000000000000000000, 0.8660254037844387076, 1.000000000000000000, 0.8660254037844387076, 1.000000000000000000, 0.8660254037844387076, 1.000000000000000000, 0.8660254037844387076, 1.000000000000000000, 0.8660254037844387076, 1.000000000000000000, 0.8660254037844387076, 1.000000000000000000, 0.8660254037844387076, 1.000000000000000000, 0.8660254037844387076, 1.000000000000000000, 0.8660254037844387076, 1.000000000000000000, 0.8660254037844387076, 1.000000000000000000, 0.8660254037844387076, 1.000000000000000000, 0.8660254037844387076, 1.000000000000000000, 0.8660254037844387076, 1.000000000000000000, 0.8660254037844387076, 1.000000000000000000, 0.8660254037844387076, 1.000000000000000000, 0.8660254037844387076, 1.000000000000000000, 0.8660254037844387076, 1.000000000000000000, 0.8660254037844387076, 1.000000000000000000, 0.8660254037844387076, 1.000000000000000000, 0.8660254037844387076, 1.000000000000000000, 0.8660254037844387076, 1.000000000000000000, 0.8660254037844387076, 1.000000000000000000, 0.8660254037844387076, 1.000000000000000000, 0.8660254037844387076, 1.000000000000000000, 0.8660254037844387076, 1.000000000000000000, 0.8660254037844387076, 1.000000000000000000, 0.8660254037844387076, 1.000000000000000000, 0.8660254037844387076, 1.000000000000000000, 0.8660254037844387076, 1.000000000000000000, 0.8660254037844387076, 1.000000000000000000, 0.8660254037844387076, 1.000000000000000000, 0.8660254037844387076, 1.000000000000000000, 0.8660254037844387076, 1.000000000000000000, 0.8660254037844387076, 1.000000000000000000, 0.8660254037844387076, 1.000000000000000000, 0.8660254037844387076, 1.000000000000000000, 0.8660254037844387076, 1.000000000000000000, 0.8660254037844387076, 1.000000000000000000, 0.8660254037844387076, 1.000000000000000000, 0.8660254037844387076, 1.000000000000000000, 0.8660254037844387076, 1.000000000000000000, 0.8660254037844387076, 1.000000000000000000, 0.8660254037844387076, 1.000000000000000000, 0.8660254037844387076, 1.000000000000000000, 0.8660254037844387076, 1.000000000000000000, 0.8660254037844387076, 1.000000000000000000, 0.8660254037844387076, 1.000000000000000000, 0.8660254037844387076, 1.000000000000000000, 0.8660254037844387076, 1.000000000000000000, 0.8660254037844387076, 1.000000000000000000, 0.8660254037844387076, 1.000000000000000000, 0.8660254037844387076, 1.000000000000000000, 0.8660254037844387076, 1.000000000000000000, 0.8660254037844387076, 1.000000000000000000, 0.8660254037844387076, 1.000000000000000000, 0.8660254037844387076, 1.000000000000000000, 0.8660254037844387076, 1.000000000000000000, 0.8660254037844387076, 1.000000000000000000, 0.8660254037844387076, 1.000000000000000000, 0.8660254037844387076, 1.000000000000000000, 0.8660254037844387076, 1.000000000000000000, 0.8660254037844387076, 1.000000000000000000, 0.8660254037844387076, 1.000000000000000000, 0.8660254037844387076, 1.000000000000000000, 0.8660254037844387076, 1.000000000000000000, 0.8660254037844387076, 1.000000000000000000, 0.8660254037844387076, 1.000000000000000000, 0.8660254037844387076, 1.000000000000000000, 0.8660254037844387076, 1.000000000000000000, 0.8660254037844387076, 1.000000000000000000, 0.8660254037844387076, 1.000000000000000000, 0.8660254037844387076, 1.000000000000000000, 0.8660254037844387076, 1.000000000000000000, 0.8660254037844387076, 1.000000000000000000, 0.8660254037844387076, 1.000000000000000000, 0.8660254037844387076, 1.000000000000000000, 0.8660254037844387076, 1.000000000000000000, 0.8660254037844387076, 1.000000000000000000, 0.8660254037844387076, 1.000000000000000000, 0.8660254037844387076, 1.000000000000000000, 0.8660254037844387076, 1.000000000000000000, 0.8660254037844387076, 1.000000000000000000, 0.8660254037844387076, 1.000000000000000000, 0.8660254037844387076, 1.000000000000000000, 0.8660254037844387076, 1.000000000000000000, 0.8660254037844387076, 1.000000000000000000, 0.8660254037844387076, 1.000000000000000000, 0.8660254037844387076, 1.000000000000000000, 0.8660254037844387076, 1.000000000000000000, 0.8660254037844387076, 1.000000000000000000, 0.8660254037844387076, 1.000000000000000000, 0.8660254037844387076, 1.000000000000000000, 0.8660254037844387076, 1.000000000000000000, 0.8660254037844387076, 1.000000000000000000, 0.8660254037844387076, 1.000000000000000000, 0.8660254037844387076, 1.000000000000000000, 0.8660254037844387076, 1.000000000000000000, 0.8660254037844387076, 1.000000000000000000, 0.8660254037844387076, 1.000000000000000000, 0.8660254037844387076, 1.000000000000000000, 0.9548846395026606704, 0.9401540804572323662 ) ) 
 REPRESENTATION_ITEM ( '' )  );
#6232 = CARTESIAN_POINT ( 'NONE',  ( -4.243569643750005227, -23.04649784258110756, -4.360839777206344081 ) ) ;
#6233 = CARTESIAN_POINT ( 'NONE',  ( -7.316366419972956336, -13.46537015260387449, 2.120294839946750720 ) ) ;
#6234 = LINE ( 'NONE', #14968, #18295 ) ;
#6235 = AXIS2_PLACEMENT_3D ( 'NONE', #2674, #13965, #12473 ) ;
#6236 = CARTESIAN_POINT ( 'NONE',  ( 2.000000000000004441, -24.06853954178204447, -16.13143356498672887 ) ) ;
#6237 = CARTESIAN_POINT ( 'NONE',  ( -10.00000000000000000, 20.99999999999999289, 2.499999999999998224 ) ) ;
#6238 = ORIENTED_EDGE ( 'NONE', *, *, #11282, .F. ) ;
#6239 = ORIENTED_EDGE ( 'NONE', *, *, #8243, .T. ) ;
#6240 = CARTESIAN_POINT ( 'NONE',  ( -4.000000000000000888, -19.65759324776559680, -3.792472546722722715 ) ) ;
#6241 = EDGE_LOOP ( 'NONE', ( #16116, #18034, #8046, #10355 ) ) ;
#6242 = CARTESIAN_POINT ( 'NONE',  ( 0.7188294034286553114, 31.25319992234354416, 2.395093729190349130 ) ) ;
#6243 =( NAMED_UNIT ( * ) SI_UNIT ( $, .STERADIAN. ) SOLID_ANGLE_UNIT ( ) );
#6244 = CARTESIAN_POINT ( 'NONE',  ( -2.121784821875005722, -28.90027551689194496, -10.58515563886426136 ) ) ;
#6245 = CARTESIAN_POINT ( 'NONE',  ( 3.518350579753631191, 19.37180007765648071, 1.080741659609802285 ) ) ;
#6246 = CARTESIAN_POINT ( 'NONE',  ( 2.399999999999999911, 2.694222958124177006E-16, -2.200000000000000178 ) ) ;
#6247 = CARTESIAN_POINT ( 'NONE',  ( -0.9964672492307999896, -9.999999999998728129, -3.740800554895127750 ) ) ;
#6248 = EDGE_CURVE ( 'NONE', #3408, #17590, #18338, .T. ) ;
#6249 = EDGE_CURVE ( 'NONE', #5913, #12253, #16465, .T. ) ;
#6250 = CIRCLE ( 'NONE', #6550, 10.00000000000000178 ) ;
#6251 = CARTESIAN_POINT ( 'NONE',  ( 4.730628863548789710E-15, -20.72523425054125212, -13.86020214003574047 ) ) ;
#6252 = FACE_OUTER_BOUND ( 'NONE', #13100, .T. ) ;
#6253 = CARTESIAN_POINT ( 'NONE',  ( -2.121784821874996396, -20.64249580861881128, -11.60629434330255982 ) ) ;
#6254 = FACE_OUTER_BOUND ( 'NONE', #14439, .T. ) ;
#6255 = LINE ( 'NONE', #11908, #8285 ) ;
#6256 = DIRECTION ( 'NONE',  ( -1.000000000000000000, -0.000000000000000000, -0.000000000000000000 ) ) ;
#6257 = CARTESIAN_POINT ( 'NONE',  ( -4.243569643749997233, -21.36634923031502353, -10.50431910885077791 ) ) ;
#6258 = EDGE_LOOP ( 'NONE', ( #12529, #18105, #15415, #912 ) ) ;
#6259 = DIRECTION ( 'NONE',  ( -0.000000000000000000, -1.000000000000000000, -0.000000000000000000 ) ) ;
#6260 = DIRECTION ( 'NONE',  ( 0.000000000000000000, 0.000000000000000000, -1.000000000000000000 ) ) ;
#6261 = CARTESIAN_POINT ( 'NONE',  ( 0.7188294034286049072, 28.74680007765648426, -2.395093729190366005 ) ) ;
#6262 = ORIENTED_EDGE ( 'NONE', *, *, #4316, .F. ) ;
#6263 = CARTESIAN_POINT ( 'NONE',  ( 2.864755990943265829, 31.99680007765647716, 2.011557305968487697 ) ) ;
#6264 = SHAPE_DEFINITION_REPRESENTATION ( #5003, #17791 ) ;
#6265 = EDGE_CURVE ( 'NONE', #14634, #11376, #17960, .T. ) ;
#6266 = CARTESIAN_POINT ( 'NONE',  ( 1.999999999999994449, -23.18351089105175333, -2.788527940300912444 ) ) ;
#6267 = CARTESIAN_POINT ( 'NONE',  ( 2.798362969681409851, 21.00319992234354416, 2.102939460078764977 ) ) ;
#6268 = ADVANCED_FACE ( 'NONE', ( #16732 ), #1239, .T. ) ;
#6269 = ORIENTED_EDGE ( 'NONE', *, *, #4387, .F. ) ;
#6270 = CARTESIAN_POINT ( 'NONE',  ( 2.121784821875004390, -19.94344952681598926, -10.60795278932534558 ) ) ;
#6271 = CARTESIAN_POINT ( 'NONE',  ( 2.211161402132902243, 17.12180007765648071, 2.942372952327172442 ) ) ;
#6272 = EDGE_CURVE ( 'NONE', #13551, #6047, #15247, .T. ) ;
#6273 = VERTEX_POINT ( 'NONE', #16821 ) ;
#6274 = COLOUR_RGB ( '',0.8941176470588234615, 0.8941176470588234615, 0.8941176470588234615 ) ;
#6275 = CARTESIAN_POINT ( 'NONE',  ( -15.00000000000000178, 10.00000000000000000, -25.00000000000000355 ) ) ;
#6276 = CARTESIAN_POINT ( 'NONE',  ( 1.300000000000000044, 0.7216878364870329410, -1.250000000000000000 ) ) ;
#6277 = CARTESIAN_POINT ( 'NONE',  ( -5.330712181944245322E-15, -28.88206442405900631, -8.423402447113588210 ) ) ;
#6278 = CIRCLE ( 'NONE', #11601, 0.9999999999999991118 ) ;
#6279 = CARTESIAN_POINT ( 'NONE',  ( 2.000000000000004441, -23.81043014542407121, -15.76281514505668113 ) ) ;
#6280 = CARTESIAN_POINT ( 'NONE',  ( 6.734712607319251809, -10.37497835385873657, 2.111428012012234401 ) ) ;
#6281 = DIRECTION ( 'NONE',  ( -0.000000000000000000, -1.000000000000000000, -0.000000000000000000 ) ) ;
#6282 = CARTESIAN_POINT ( 'NONE',  ( -4.243569643749997233, -18.55940954492211503, -6.495593792111509224 ) ) ;
#6283 = ORIENTED_EDGE ( 'NONE', *, *, #1701, .T. ) ;
#6284 = DIRECTION ( 'NONE',  ( 0.000000000000000000, 0.000000000000000000, 1.000000000000000000 ) ) ;
#6285 = CIRCLE ( 'NONE', #7762, 0.9999999999999991118 ) ;
#6286 = CARTESIAN_POINT ( 'NONE',  ( -5.279047395330986450E-15, -26.47387988119159985, -5.474502901475981176 ) ) ;
#6287 = AXIS2_PLACEMENT_3D ( 'NONE', #13075, #3263, #669 ) ;
#6288 = VERTEX_POINT ( 'NONE', #2541 ) ;
#6289 = ORIENTED_EDGE ( 'NONE', *, *, #14069, .T. ) ;
#6290 = DIRECTION ( 'NONE',  ( 0.000000000000000000, 0.000000000000000000, 1.000000000000000000 ) ) ;
#6291 = DIRECTION ( 'NONE',  ( -0.000000000000000000, -0.5735764363510414965, -0.8191520442889950182 ) ) ;
#6292 =( NAMED_UNIT ( * ) SI_UNIT ( $, .STERADIAN. ) SOLID_ANGLE_UNIT ( ) );
#6293 = CARTESIAN_POINT ( 'NONE',  ( -1.444289557195956863, 24.00319992234354416, 4.262301884875733471 ) ) ;
#6294 = EDGE_CURVE ( 'NONE', #16052, #7494, #9054, .T. ) ;
#6295 = CARTESIAN_POINT ( 'NONE',  ( 2.211161402132839182, 32.87819992234354771, -2.942372952327217739 ) ) ;
#6296 = CARTESIAN_POINT ( 'NONE',  ( -1.593127413382952939, 16.62819992234354061, 2.091722143975172532 ) ) ;
#6297 = EDGE_LOOP ( 'NONE', ( #2091, #503, #1853, #11768 ) ) ;
#6298 = CARTESIAN_POINT ( 'NONE',  ( 1.336863392178479160, 18.74680007765647005, -4.297206761780677731 ) ) ;
#6299 = PRODUCT_RELATED_PRODUCT_CATEGORY ( 'part', '', ( #16425 ) ) ;
#6300 = CARTESIAN_POINT ( 'NONE',  ( 1.999999999999994449, -25.44196810847903478, -6.013939113682064352 ) ) ;
#6301 = VERTEX_POINT ( 'NONE', #12710 ) ;
#6302 = CIRCLE ( 'NONE', #14279, 0.9999999999999991118 ) ;
#6303 = DIRECTION ( 'NONE',  ( -1.214671430232282197E-14, -0.8191520442889844711, 0.5735764363510568176 ) ) ;
#6304 = AXIS2_PLACEMENT_3D ( 'NONE', #7485, #9830, #362 ) ;
#6305 = CARTESIAN_POINT ( 'NONE',  ( 2.864755990943265829, 36.99680007765648071, 2.011557305968487697 ) ) ;
#6306 = CARTESIAN_POINT ( 'NONE',  ( 20.00000000000000355, 4.052968581778165278E-16, -3.309499999999999886 ) ) ;
#6307 = APPLICATION_CONTEXT ( 'automotive_design' ) ;
#6308 = CARTESIAN_POINT ( 'NONE',  ( 4.243569643750000786, -19.86730713195397868, -4.091975012412500945 ) ) ;
#6309 = CARTESIAN_POINT ( 'NONE',  ( -4.243569643750000786, -24.15837584640520674, -10.22025624374954766 ) ) ;
#6310 = FACE_BOUND ( 'NONE', #8681, .T. ) ;
#6311 = ORIENTED_EDGE ( 'NONE', *, *, #7424, .F. ) ;
#6312 = CARTESIAN_POINT ( 'NONE',  ( 0.6435604995507229198, -10.54254386713301628, 22.30101802474215233 ) ) ;
#6313 = CARTESIAN_POINT ( 'NONE',  ( 10.00000000000000355, 34.19999999999999574, 2.499999999999996891 ) ) ;
#6314 = CIRCLE ( 'NONE', #1280, 0.9999999999999991118 ) ;
#6315 = CARTESIAN_POINT ( 'NONE',  ( 2.399999999999999911, 0.000000000000000000, 0.000000000000000000 ) ) ;
#6316 = CARTESIAN_POINT ( 'NONE',  ( -4.243569643750005227, -28.72490456245641965, -12.47044501566739427 ) ) ;
#6317 = ORIENTED_EDGE ( 'NONE', *, *, #16020, .F. ) ;
#6318 = CIRCLE ( 'NONE', #3644, 10.00000000000000000 ) ;
#6319 = CARTESIAN_POINT ( 'NONE',  ( -3.518350579753605434, 24.37819992234353705, 1.080741659609877781 ) ) ;
#6320 = CARTESIAN_POINT ( 'NONE',  ( 9.000000000000005329, -10.00000000000000000, -3.713574246709344884 ) ) ;
#6321 = CARTESIAN_POINT ( 'NONE',  ( -2.121784821875005722, -25.02863457152241722, -5.055879339913546211 ) ) ;
#6322 = CARTESIAN_POINT ( 'NONE',  ( -0.05938372350926768989, 23.62180007765648071, -2.628655560595669183 ) ) ;
#6323 = EDGE_CURVE ( 'NONE', #12786, #2131, #14704, .T. ) ;
#6324 = CARTESIAN_POINT ( 'NONE',  ( 2.829195390882724759, 20.37819992234354416, -3.793023760679264278 ) ) ;
#6325 = CARTESIAN_POINT ( 'NONE',  ( 2.000000000000004441, -16.90600379355336003, -5.902272412934671308 ) ) ;
#6326 = CARTESIAN_POINT ( 'NONE',  ( 3.999999999999996447, -27.57189644185653066, -11.06895097103799763 ) ) ;
#6327 = EDGE_CURVE ( 'NONE', #9609, #1200, #2561, .T. ) ;
#6328 = CARTESIAN_POINT ( 'NONE',  ( 4.730628863548789710E-15, -17.36981209788766378, -9.068162680945119902 ) ) ;
#6329 = EDGE_CURVE ( 'NONE', #16354, #14538, #11125, .T. ) ;
#6330 = CARTESIAN_POINT ( 'NONE',  ( -4.518350579753632523, 35.62180007765647360, -1.405661355842698468 ) ) ;
#6331 = AXIS2_PLACEMENT_3D ( 'NONE', #10056, #1466, #7190 ) ;
#6332 = DIRECTION ( 'NONE',  ( -0.000000000000000000, -1.000000000000000000, -0.000000000000000000 ) ) ;
#6333 = LINE ( 'NONE', #14786, #15431 ) ;
#6334 = CARTESIAN_POINT ( 'NONE',  ( 3.999999999999996447, -24.53911103535534366, -6.737684537866703849 ) ) ;
#6335 = ORIENTED_EDGE ( 'NONE', *, *, #16935, .T. ) ;
#6336 = ORIENTED_EDGE ( 'NONE', *, *, #15316, .T. ) ;
#6337 = CARTESIAN_POINT ( 'NONE',  ( 8.500000000000001776, 15.00000000000000178, -22.64999999999999147 ) ) ;
#6338 = DIRECTION ( 'NONE',  ( 0.000000000000000000, 0.000000000000000000, 1.000000000000000000 ) ) ;
#6339 = DIRECTION ( 'NONE',  ( 0.000000000000000000, 0.8191520442889952403, -0.5735764363510413855 ) ) ;
#6340 = ORIENTED_EDGE ( 'NONE', *, *, #12494, .F. ) ;
#6341 = CARTESIAN_POINT ( 'NONE',  ( 2.518350579753611207, 30.62819992234355126, -0.7558219633769606149 ) ) ;
#6342 =( NAMED_UNIT ( * ) PLANE_ANGLE_UNIT ( ) SI_UNIT ( $, .RADIAN. ) );
#6343 = CARTESIAN_POINT ( 'NONE',  ( 4.243569643749996345, -27.83227623338511947, -11.19563964674263978 ) ) ;
#6344 = CARTESIAN_POINT ( 'NONE',  ( -3.500000000000000444, 20.49680007765647716, 0.05647727720536892260 ) ) ;
#6345 =( BOUNDED_CURVE ( )  B_SPLINE_CURVE ( 2, ( #7756, #6373, #541, #4700, #1944, #14643, #6279, #7570, #16211 ),
 .UNSPECIFIED., .F., .T. ) 
 B_SPLINE_CURVE_WITH_KNOTS ( ( 3, 2, 2, 2, 3 ),
 ( 0.06034482758620690612, 0.06321839080459770721, 0.06896551724137930939, 0.07471264367816092544, 0.07758620689655172653 ),
 .UNSPECIFIED. ) 
 CURVE ( )  GEOMETRIC_REPRESENTATION_ITEM ( )  RATIONAL_B_SPLINE_CURVE ( ( 0.9330127018922194093, 0.9330127018922195203, 1.000000000000000000, 0.8660254037844387076, 1.000000000000000000, 0.8660254037844387076, 1.000000000000000000, 0.9330127018922194093, 0.9330127018922194093 ) ) 
 REPRESENTATION_ITEM ( '' )  );
#6346 = TOROIDAL_SURFACE ( 'NONE', #15237, 4.400000000000002132, 0.4000000000000000222 ) ;
#6347 = DIRECTION ( 'NONE',  ( -0.000000000000000000, -1.000000000000000000, -0.000000000000000000 ) ) ;
#6348 = CARTESIAN_POINT ( 'NONE',  ( 3.973088838427932590, -15.08697326462720056, -8.369503528065322939 ) ) ;
#6349 = EDGE_CURVE ( 'NONE', #15303, #9997, #6975, .T. ) ;
#6350 = CARTESIAN_POINT ( 'NONE',  ( -4.243569643749997233, -22.94726928300758217, -12.76210693092232162 ) ) ;
#6351 = DIRECTION ( 'NONE',  ( 0.000000000000000000, 0.000000000000000000, -1.000000000000000000 ) ) ;
#6352 = CARTESIAN_POINT ( 'NONE',  ( -1.999999999999996225, -17.37920435354295989, -6.578072849473089789 ) ) ;
#6353 = DIRECTION ( 'NONE',  ( 0.000000000000000000, 0.000000000000000000, 1.000000000000000000 ) ) ;
#6354 = CARTESIAN_POINT ( 'NONE',  ( -4.243569643750005227, -25.33721873525807666, -7.632328254085517294 ) ) ;
#6355=STYLED_ITEM('',(#18396),#8351);
#6356 = ORIENTED_EDGE ( 'NONE', *, *, #13216, .T. ) ;
#6357 = CARTESIAN_POINT ( 'NONE',  ( 3.885274725274725949, -4.336808689942017736E-16, 0.000000000000000000 ) ) ;
#6358 = LINE ( 'NONE', #4776, #2941 ) ;
#6359 = CARTESIAN_POINT ( 'NONE',  ( 2.500000000000001332, 31.74680007765648782, -0.05647727720535888202 ) ) ;
#6360 = VERTEX_POINT ( 'NONE', #18131 ) ;
#6361 = CARTESIAN_POINT ( 'NONE',  ( -1.135272562821090014, 28.49680007765648071, -3.311245368580554072 ) ) ;
#6362 = ADVANCED_FACE ( 'NONE', ( #8174 ), #13931, .F. ) ;
#6363 = DIRECTION ( 'NONE',  ( 0.000000000000000000, 0.8191520442889952403, -0.5735764363510413855 ) ) ;
#6364 = APPLICATION_PROTOCOL_DEFINITION ( 'draft international standard', 'automotive_design', 1998, #10071 ) ;
#6365 = DIRECTION ( 'NONE',  ( 0.000000000000000000, 0.000000000000000000, -1.000000000000000000 ) ) ;
#6366 = VERTEX_POINT ( 'NONE', #5489 ) ;
#6367 = CARTESIAN_POINT ( 'NONE',  ( -4.243569643749998122, -20.36617531942789938, -9.075922731621842487 ) ) ;
#6368 = CARTESIAN_POINT ( 'NONE',  ( 1.027846397803542144, 16.24680007765647716, -3.346150245485522312 ) ) ;
#6369 = ORIENTED_EDGE ( 'NONE', *, *, #10366, .T. ) ;
#6370 = CARTESIAN_POINT ( 'NONE',  ( 0.000000000000000000, 13.00000000000000178, 0.000000000000000000 ) ) ;
#6371 = CARTESIAN_POINT ( 'NONE',  ( 0.000000000000000000, 18.79999999999999361, 2.500000000000000000 ) ) ;
#6372 = DIRECTION ( 'NONE',  ( 0.000000000000000000, 0.000000000000000000, -1.000000000000000000 ) ) ;
#6373 = CARTESIAN_POINT ( 'NONE',  ( 1.071796769724487675, -30.02068312334193934, -11.61871151373218503 ) ) ;
#6374 = CARTESIAN_POINT ( 'NONE',  ( 6.428571428571432378, -14.26578344203647930, -2.827263138854382074 ) ) ;
#6375 = CARTESIAN_POINT ( 'NONE',  ( -3.999999999999997335, -23.14312172474173224, -12.79664100063768650 ) ) ;
#6376 = CARTESIAN_POINT ( 'NONE',  ( -4.243569643750000786, -20.02862550467770220, -4.322361524868783889 ) ) ;
#6377 = ADVANCED_FACE ( 'NONE', ( #16 ), #8439, .T. ) ;
#6378 = VERTEX_POINT ( 'NONE', #4096 ) ;
#6379 = CARTESIAN_POINT ( 'NONE',  ( 1.300000000000000044, -0.7216878364870317197, 1.250000000000000000 ) ) ;
#6380 = CARTESIAN_POINT ( 'NONE',  ( 4.000000000000000888, -22.62585130588224658, -8.031584375918267682 ) ) ;
#6381 = EDGE_CURVE ( 'NONE', #1052, #18219, #17124, .T. ) ;
#6382 = VERTEX_POINT ( 'NONE', #5308 ) ;
#6383 = VERTEX_POINT ( 'NONE', #10866 ) ;
#6384 = SURFACE_STYLE_USAGE ( .BOTH. , #12028 ) ;
#6385 =( NAMED_UNIT ( * ) SI_UNIT ( $, .STERADIAN. ) SOLID_ANGLE_UNIT ( ) );
#6386 = ADVANCED_FACE ( 'NONE', ( #10959 ), #9933, .F. ) ;
#6387 = CARTESIAN_POINT ( 'NONE',  ( -2.733110507866328476, 27.37819992234355126, -3.862833514489096398 ) ) ;
#6388 = CARTESIAN_POINT ( 'NONE',  ( -3.481649420246394566, 37.12819992234354061, -1.193696214020467883 ) ) ;
#6389 = CARTESIAN_POINT ( 'NONE',  ( 1.593127413382953383, 20.37819992234354771, -2.091722143975172532 ) ) ;
#6390 = EDGE_LOOP ( 'NONE', ( #1615, #17715, #10169, #16601 ) ) ;
#6391 = ADVANCED_FACE ( 'NONE', ( #4189 ), #13835, .T. ) ;
#6392 = CARTESIAN_POINT ( 'NONE',  ( 4.499999999999999112, 38.25319992234354061, 0.05647727720528474687 ) ) ;
#6393 = CARTESIAN_POINT ( 'NONE',  ( 4.713407268011036227E-15, -18.71329538077844390, -10.49651124437128225 ) ) ;
#6394 = EDGE_LOOP ( 'NONE', ( #15128, #473, #13236, #6661 ) ) ;
#6395 = CARTESIAN_POINT ( 'NONE',  ( -11.99999999999999822, 48.00000000000000000, -15.00000000000000000 ) ) ;
#6396 = CARTESIAN_POINT ( 'NONE',  ( 2.211161402132902243, 37.12180007765645939, 2.942372952327172442 ) ) ;
#6397 = CYLINDRICAL_SURFACE ( 'NONE', #12631, 2.000000000000001776 ) ;
#6398 = CARTESIAN_POINT ( 'NONE',  ( -4.243569643749998122, -17.75281768130346194, -5.343661229830111381 ) ) ;
#6399 = CARTESIAN_POINT ( 'NONE',  ( -2.121784821875005722, -26.86766402057294556, -7.682285581915135886 ) ) ;
#6400 = CARTESIAN_POINT ( 'NONE',  ( -4.648177544792955347E-16, -29.83862777749724060, -11.35870953444733011 ) ) ;
#6401 = VERTEX_POINT ( 'NONE', #2553 ) ;
#6402 = AXIS2_PLACEMENT_3D ( 'NONE', #12770, #73, #2126 ) ;
#6403 = CARTESIAN_POINT ( 'NONE',  ( -1.071796769724486786, -16.62756776554380878, -6.438934876394256435 ) ) ;
#6404 = LINE ( 'NONE', #5190, #17598 ) ;
#6405 = CARTESIAN_POINT ( 'NONE',  ( -4.433153569487539691, -10.00000000000000000, 28.39434458091831459 ) ) ;
#6406 = CARTESIAN_POINT ( 'NONE',  ( 2.121784821875004390, -23.29887167946958115, -15.39999224841596437 ) ) ;
#6407 = ORIENTED_EDGE ( 'NONE', *, *, #10920, .F. ) ;
#6408 = CARTESIAN_POINT ( 'NONE',  ( 0.05938372350920109732, 27.62819992234353705, -3.680117784833935701 ) ) ;
#6409 = FACE_BOUND ( 'NONE', #2619, .T. ) ;
#6410 = CARTESIAN_POINT ( 'NONE',  ( 4.730628863548789710E-15, -17.33754842334290913, -9.022085378453862603 ) ) ;
#6411 = CARTESIAN_POINT ( 'NONE',  ( -2.055738996568313048, 25.74680007765648426, -1.423772053676023441 ) ) ;
#6412 = CARTESIAN_POINT ( 'NONE',  ( -4.499999999999999112, 19.50319992234354416, -0.05647727720528529505 ) ) ;
#6413 = CARTESIAN_POINT ( 'NONE',  ( 4.730628863548789710E-15, -21.75767183597313092, -15.33467581975593141 ) ) ;
#6414 = CARTESIAN_POINT ( 'NONE',  ( -3.999999999999997335, -24.69177810288953978, -15.00835152021797114 ) ) ;
#6415 = CARTESIAN_POINT ( 'NONE',  ( 4.243569643749996345, -23.73478956620236957, -5.343822230353133307 ) ) ;
#6416 = VECTOR ( 'NONE', #17319, 1000.000000000000000 ) ;
#6417 = CARTESIAN_POINT ( 'NONE',  ( 3.607379964056306676, 36.49680007765646650, -2.690724712371305838 ) ) ;
#6418 = CARTESIAN_POINT ( 'NONE',  ( -8.500000000000010658, 14.80000000000000071, 18.29999999999999005 ) ) ;
#6419 = DIRECTION ( 'NONE',  ( -0.000000000000000000, 0.5000000000000002220, -0.8660254037844384856 ) ) ;
#6420 = CARTESIAN_POINT ( 'NONE',  ( 4.000000000000000888, -22.62585130588224658, -8.031584375918267682 ) ) ;
#6421 = ORIENTED_EDGE ( 'NONE', *, *, #5479, .F. ) ;
#6422 = ORIENTED_EDGE ( 'NONE', *, *, #13298, .F. ) ;
#6423 = CARTESIAN_POINT ( 'NONE',  ( 4.898587196589413815E-16, 2.700915433685006750, 35.11257424290206330 ) ) ;
#6424 = CARTESIAN_POINT ( 'NONE',  ( -5.577813053751546416E-15, -24.67643985033786791, -3.986341135846375838 ) ) ;
#6425 = CARTESIAN_POINT ( 'NONE',  ( 0.000000000000000000, 13.00000000000000178, 0.000000000000000000 ) ) ;
#6426 = ORIENTED_EDGE ( 'NONE', *, *, #1184, .T. ) ;
#6427 = CARTESIAN_POINT ( 'NONE',  ( -0.7188294034286550893, 25.00319992234354771, -2.395093729190349130 ) ) ;
#6428 = DIRECTION ( 'NONE',  ( 1.000000000000000000, 0.000000000000000000, 0.000000000000000000 ) ) ;
#6429 = CIRCLE ( 'NONE', #10262, 10.00000000000000000 ) ;
#6430 = CARTESIAN_POINT ( 'NONE',  ( -4.243569643749997233, -22.91500560846283463, -12.71602962843106432 ) ) ;
#6431 = CARTESIAN_POINT ( 'NONE',  ( 2.798362969681366330, 21.49680007765647716, -2.102939460078824929 ) ) ;
#6432 = ADVANCED_FACE ( 'NONE', ( #976 ), #15437, .T. ) ;
#6433 = FACE_OUTER_BOUND ( 'NONE', #2336, .T. ) ;
#6434 = CARTESIAN_POINT ( 'NONE',  ( -4.000000000000004441, -25.85116713280339340, -8.611494838171019239 ) ) ;
#6435 = CARTESIAN_POINT ( 'NONE',  ( 2.121784821874994176, -28.37330216599443489, -9.832559698173744422 ) ) ;
#6436 = VECTOR ( 'NONE', #10934, 1000.000000000000000 ) ;
#6437 = TOROIDAL_SURFACE ( 'NONE', #14436, 9.000000000000001776, 0.9999999999999991118 ) ;
#6438 = FACE_BOUND ( 'NONE', #9250, .T. ) ;
#6439 = CARTESIAN_POINT ( 'NONE',  ( 0.000000000000000000, 3.000000000000000000, 0.000000000000000000 ) ) ;
#6440 = CARTESIAN_POINT ( 'NONE',  ( 9.000000000000001776, 36.39999999999999147, -2.500000000000002665 ) ) ;
#6441 = CARTESIAN_POINT ( 'NONE',  ( 4.243569643749996345, -25.50929166616339572, -7.878073867372210159 ) ) ;
#6442 = ORIENTED_EDGE ( 'NONE', *, *, #13039, .T. ) ;
#6443 = CARTESIAN_POINT ( 'NONE',  ( 14.99999999999999822, 13.00000000000000178, 24.99999999999999645 ) ) ;
#6444 = LINE ( 'NONE', #17694, #15383 ) ;
#6445 = CARTESIAN_POINT ( 'NONE',  ( -1.593127413382998459, 30.87180007765647716, -2.091722143975139669 ) ) ;
#6446 = ADVANCED_FACE ( 'NONE', ( #16457 ), #14029, .T. ) ;
#6447 = ORIENTED_EDGE ( 'NONE', *, *, #15347, .T. ) ;
#6448 = CARTESIAN_POINT ( 'NONE',  ( -2.115076519116362519, 32.62180007765647360, 3.012182706137108035 ) ) ;
#6449 = CLOSED_SHELL ( 'NONE', ( #16693, #13726, #16253, #5082, #3144, #15149, #3995, #15963, #7780, #14463, #2550, #263, #15398 ) ) ;
#6450 = CARTESIAN_POINT ( 'NONE',  ( 4.000000000000000000, -1.759474945355381292, 3.047500000000002540 ) ) ;
#6451 = VECTOR ( 'NONE', #15266, 1000.000000000000000 ) ;
#6452 = VECTOR ( 'NONE', #11532, 1000.000000000000000 ) ;
#6453 = ORIENTED_EDGE ( 'NONE', *, *, #13386, .T. ) ;
#6454 = CARTESIAN_POINT ( 'NONE',  ( -2.121784821874996396, -19.64232189773168358, -10.17789796607362618 ) ) ;
#6455 = CARTESIAN_POINT ( 'NONE',  ( 3.500000000000000444, 21.74680007765647716, -0.05647727720536935281 ) ) ;
#6456 = ORIENTED_EDGE ( 'NONE', *, *, #612, .F. ) ;
#6457 = DIRECTION ( 'NONE',  ( 0.000000000000000000, 0.000000000000000000, 1.000000000000000000 ) ) ;
#6458 = CARTESIAN_POINT ( 'NONE',  ( -1.840775681772796268, -24.12649185032508825, -16.50800845489187196 ) ) ;
#6459 = CIRCLE ( 'NONE', #15636, 10.00000000000000000 ) ;
#6460 = CARTESIAN_POINT ( 'NONE',  ( 9.666809584889323403, -9.963386536547416128, 0.1573640763989413160 ) ) ;
#6462 = DIRECTION ( 'NONE',  ( 0.000000000000000000, 0.000000000000000000, 1.000000000000000000 ) ) ;
#6461 = AXIS2_PLACEMENT_3D ( 'NONE', #3282, #4566, #1992 ) ;
#6463 = CARTESIAN_POINT ( 'NONE',  ( -5.330712181944245322E-15, -23.97798589325759977, -1.419652468442682558 ) ) ;
#6464 = EDGE_LOOP ( 'NONE', ( #10886, #4881, #7225, #4869 ) ) ;
#6465 = CARTESIAN_POINT ( 'NONE',  ( -9.184850993605147944E-16, 43.00000000000000000, -2.500000000000000000 ) ) ;
#6466 = CARTESIAN_POINT ( 'NONE',  ( -5.279047395330986450E-15, -26.99009867390753925, -6.211739741336077536 ) ) ;
#6467 = CARTESIAN_POINT ( 'NONE',  ( 3.518350579753631191, 34.37180007765648071, 1.080741659609802285 ) ) ;
#6468 = ORIENTED_EDGE ( 'NONE', *, *, #10633, .T. ) ;
#6469 = ORIENTED_EDGE ( 'NONE', *, *, #10045, .T. ) ;
#6470 = CARTESIAN_POINT ( 'NONE',  ( -1.336863392178569088, 35.00319992234354771, -4.297206761780648421 ) ) ;
#6471 = CARTESIAN_POINT ( 'NONE',  ( 3.518350579753606322, 33.12819992234354771, -1.080741659609876892 ) ) ;
#6472 = CARTESIAN_POINT ( 'NONE',  ( 2.518350579753611207, 25.62819992234354416, -0.7558219633769606149 ) ) ;
#6473 = ORIENTED_EDGE ( 'NONE', *, *, #10561, .F. ) ;
#6474 = CARTESIAN_POINT ( 'NONE',  ( 2.733110507866247652, 21.37180007765647360, -3.862833514489153686 ) ) ;
#6475 = VECTOR ( 'NONE', #14480, 1000.000000000000227 ) ;
#6476 = CARTESIAN_POINT ( 'NONE',  ( -5.279047395330986450E-15, -24.34447736053341416, -2.433400936046320684 ) ) ;
#6477 = EDGE_LOOP ( 'NONE', ( #15112, #7532, #533, #13690 ) ) ;
#6478 = EDGE_CURVE ( 'NONE', #8773, #12774, #6699, .T. ) ;
#6479 = DIRECTION ( 'NONE',  ( 0.000000000000000000, -1.000000000000000000, 0.000000000000000000 ) ) ;
#6480 = ADVANCED_FACE ( 'NONE', ( #8092 ), #8454, .T. ) ;
#6481 = CARTESIAN_POINT ( 'NONE',  ( 0.05938372350927906274, 37.37180007765645939, 3.680117784833935701 ) ) ;
#6482 = DIRECTION ( 'NONE',  ( 0.9454169814551710571, 0.000000000000000000, 0.3258630558627237384 ) ) ;
#6483 = EDGE_CURVE ( 'NONE', #13448, #10757, #8927, .T. ) ;
#6484 = CARTESIAN_POINT ( 'NONE',  ( -2.121784821874996396, -17.80329244868115168, -7.551491724072033840 ) ) ;
#6485 = CARTESIAN_POINT ( 'NONE',  ( 4.243569643749996345, -25.79966473706612007, -8.292769589793513418 ) ) ;
#6486 = PRODUCT ( 'Coil Housing', 'Coil Housing', '', ( #17700 ) ) ;
#6487 = ADVANCED_FACE ( 'NONE', ( #5498 ), #10972, .F. ) ;
#6488 = AXIS2_PLACEMENT_3D ( 'NONE', #3682, #17886, #13324 ) ;
#6489 = CARTESIAN_POINT ( 'NONE',  ( 1.907117511807822519, -29.88501818502292906, -12.24335744624743860 ) ) ;
#6490 = ORIENTED_EDGE ( 'NONE', *, *, #3723, .T. ) ;
#6491 = PRODUCT_DEFINITION_CONTEXT ( 'detailed design', #6987, 'design' ) ;
#6492 = CARTESIAN_POINT ( 'NONE',  ( 7.191589934391298122, -10.00000000000000178, 14.52136967842653981 ) ) ;
#6493 = DIRECTION ( 'NONE',  ( -0.000000000000000000, 1.000000000000000000, -0.000000000000000000 ) ) ;
#6494 = CARTESIAN_POINT ( 'NONE',  ( 1.071796769724476128, -18.78002368763965890, -9.512960511135750252 ) ) ;
#6495 = CARTESIAN_POINT ( 'NONE',  ( -4.243569643749997233, -24.75403505751336297, -15.34243587043265755 ) ) ;
#6496 = ORIENTED_EDGE ( 'NONE', *, *, #1381, .F. ) ;
#6497 = CARTESIAN_POINT ( 'NONE',  ( 0.05938372350920109732, 37.62819992234352640, -3.680117784833935701 ) ) ;
#6498 = ADVANCED_BREP_SHAPE_REPRESENTATION ( '', ( #13901, #16940 ), #12175 ) ;
#6499 = CARTESIAN_POINT ( 'NONE',  ( 3.694449856179180092, -25.69578722143081251, -15.18691654432904947 ) ) ;
#6500 = CARTESIAN_POINT ( 'NONE',  ( -4.243569643749997233, -18.26903647401939779, -6.080898069690205965 ) ) ;
#6501 = CARTESIAN_POINT ( 'NONE',  ( -1.593127413382998459, 18.37180007765648071, -2.091722143975139669 ) ) ;
#6502 = CARTESIAN_POINT ( 'NONE',  ( 1.336863392178569754, 18.75319992234354416, 4.297206761780648421 ) ) ;
#6503 = CARTESIAN_POINT ( 'NONE',  ( 2.000000000000004441, -22.51988316363423337, -13.91972304540644245 ) ) ;
#6504 = ORIENTED_EDGE ( 'NONE', *, *, #16945, .F. ) ;
#6505 = CIRCLE ( 'NONE', #11233, 2.000000000000001776 ) ;
#6506 = CARTESIAN_POINT ( 'NONE',  ( 4.243569643750003451, -19.67788359580665869, -8.092940278475046156 ) ) ;
#6507=STYLED_ITEM('',(#18396),#7672);
#6508 = CARTESIAN_POINT ( 'NONE',  ( -1.444289557196047014, 38.49680007765647360, -4.262301884875704161 ) ) ;
#6509 = DIRECTION ( 'NONE',  ( 0.000000000000000000, 0.000000000000000000, -1.000000000000000000 ) ) ;
#6510 = CARTESIAN_POINT ( 'NONE',  ( 0.000000000000000000, -15.45745613286697839, -10.86990606519494129 ) ) ;
#6511 = AXIS2_PLACEMENT_3D ( 'NONE', #8920, #5031, #10686 ) ;
#6512 = DIRECTION ( 'NONE',  ( 0.000000000000000000, 0.000000000000000000, -1.000000000000000000 ) ) ;
#6513 = ORIENTED_EDGE ( 'NONE', *, *, #2527, .T. ) ;
#6514 = VERTEX_POINT ( 'NONE', #3926 ) ;
#6515 = DIRECTION ( 'NONE',  ( 3.469446951953612217E-16, -0.000000000000000000, 1.000000000000000000 ) ) ;
#6516 = CARTESIAN_POINT ( 'NONE',  ( 2.000000000000004441, -18.71276956805914082, -8.482601352445005460 ) ) ;
#6517 = CARTESIAN_POINT ( 'NONE',  ( 0.000000000000000000, 3.771166001944911361, 16.59141230903429687 ) ) ;
#6518 = ORIENTED_EDGE ( 'NONE', *, *, #9660, .F. ) ;
#6519 = CARTESIAN_POINT ( 'NONE',  ( 2.055738996568281518, 28.00319992234354771, -1.423772053676066518 ) ) ;
#6520 = CARTESIAN_POINT ( 'NONE',  ( -2.121784821875005722, -27.35161913874413386, -8.373445119283974947 ) ) ;
#6521 = CARTESIAN_POINT ( 'NONE',  ( 3.500000000000000444, 21.74680007765647716, -0.05647727720536935281 ) ) ;
#6522 = DIRECTION ( 'NONE',  ( -0.000000000000000000, -1.000000000000000000, -0.000000000000000000 ) ) ;
#6523 = CARTESIAN_POINT ( 'NONE',  ( 4.371749249414307315, -10.00000000000000178, -10.94697576041283682 ) ) ;
#6524 = CARTESIAN_POINT ( 'NONE',  ( -5.330712181944245322E-15, -29.65639261313291541, -9.529257706903733194 ) ) ;
#6525 = AXIS2_PLACEMENT_3D ( 'NONE', #11130, #18300, #4086 ) ;
#6526 = CIRCLE ( 'NONE', #12457, 4.000000000000000000 ) ;
#6527 = DIRECTION ( 'NONE',  ( -0.000000000000000000, 1.000000000000000000, 1.224646799147353207E-16 ) ) ;
#6528 = CARTESIAN_POINT ( 'NONE',  ( 4.499999999999999112, 24.24680007765647716, -0.05647727720537982360 ) ) ;
#6529 = DIRECTION ( 'NONE',  ( -1.000000000000000000, 0.000000000000000000, 0.000000000000000000 ) ) ;
#6530 = DIRECTION ( 'NONE',  ( 0.000000000000000000, 0.000000000000000000, 1.000000000000000000 ) ) ;
#6531 = CARTESIAN_POINT ( 'NONE',  ( -2.121784821875005722, -25.02863457152241722, -5.055879339913546211 ) ) ;
#6532 = FACE_OUTER_BOUND ( 'NONE', #17800, .T. ) ;
#6533 = PLANE ( 'NONE',  #12716 ) ;
#6534 = CARTESIAN_POINT ( 'NONE',  ( 3.999999999999996447, -27.12020499893503001, -10.42386873716718121 ) ) ;
#6535 = CARTESIAN_POINT ( 'NONE',  ( 1.989345975306426206, 31.49680007765648071, -1.515154207786343799 ) ) ;
#6536 = EDGE_LOOP ( 'NONE', ( #16909, #10177 ) ) ;
#6537 = CARTESIAN_POINT ( 'NONE',  ( 0.05938372350927906967, 27.37180007765647716, 3.680117784833935701 ) ) ;
#6538 = CARTESIAN_POINT ( 'NONE',  ( -4.648177544792955347E-16, -29.83862777749724060, -11.35870953444733011 ) ) ;
#6539 = AXIS2_PLACEMENT_3D ( 'NONE', #6067, #1729, #3302 ) ;
#6540 = DIRECTION ( 'NONE',  ( -0.000000000000000000, 1.000000000000000000, -0.000000000000000000 ) ) ;
#6541 = ORIENTED_EDGE ( 'NONE', *, *, #5595, .F. ) ;
#6542 = CARTESIAN_POINT ( 'NONE',  ( -4.243569643750000786, -22.86782886461536179, -8.377164144099308984 ) ) ;
#6543 = CARTESIAN_POINT ( 'NONE',  ( -1.135272562821090014, 25.99680007765648071, -3.311245368580554072 ) ) ;
#6544 = ORIENTED_EDGE ( 'NONE', *, *, #11117, .F. ) ;
#6545 = ADVANCED_FACE ( 'NONE', ( #15257 ), #16835, .T. ) ;
#6546 = CARTESIAN_POINT ( 'NONE',  ( 0.000000000000000000, 33.00000000000000000, 5.000000000000000000 ) ) ;
#6547 = ADVANCED_FACE ( 'NONE', ( #1338 ), #8001, .F. ) ;
#6548 = DIRECTION ( 'NONE',  ( 0.000000000000000000, 0.5000000000000011102, 0.8660254037844380415 ) ) ;
#6549 = CARTESIAN_POINT ( 'NONE',  ( 1.261028757266463796, -23.92767164650701872, -16.69611796327299658 ) ) ;
#6550 = AXIS2_PLACEMENT_3D ( 'NONE', #3397, #891, #13483 ) ;
#6551 = CARTESIAN_POINT ( 'NONE',  ( 9.889275785751310721, -9.933886151507580919, 2.519662976721114944 ) ) ;
#6552 = EDGE_CURVE ( 'NONE', #17766, #3719, #14095, .T. ) ;
#6553 = CARTESIAN_POINT ( 'NONE',  ( 3.579096709490575479E-14, -24.93454924669583406, -4.354959555776423130 ) ) ;
#6554 = CARTESIAN_POINT ( 'NONE',  ( 2.121784821874994176, -22.95300484247709250, -2.091572879642740634 ) ) ;
#6555 = EDGE_LOOP ( 'NONE', ( #10273, #2787, #3013, #2135 ) ) ;
#6556 = FACE_OUTER_BOUND ( 'NONE', #9251, .T. ) ;
#6557 = CARTESIAN_POINT ( 'NONE',  ( -1.999999999999996225, -20.47651710983858564, -11.00149388863366440 ) ) ;
#6558 = CARTESIAN_POINT ( 'NONE',  ( -2.798362969681365886, 30.24680007765648071, 2.102939460078824929 ) ) ;
#6559 = ORIENTED_EDGE ( 'NONE', *, *, #5747, .T. ) ;
#6560 = VERTEX_POINT ( 'NONE', #13843 ) ;
#6561 = CARTESIAN_POINT ( 'NONE',  ( -1.999999999999996225, -18.34711458918039995, -7.960391923204007014 ) ) ;
#6562 = CARTESIAN_POINT ( 'NONE',  ( -4.518350579753602325, 31.87819992234354416, 1.405661355842794391 ) ) ;
#6563 = CARTESIAN_POINT ( 'NONE',  ( 3.999999999999996447, -25.50702127099278371, -8.120003611597617521 ) ) ;
#6564 = CARTESIAN_POINT ( 'NONE',  ( -1.497042530366522461, 29.87819992234354416, -2.161531897785030409 ) ) ;
#6565 = ORIENTED_EDGE ( 'NONE', *, *, #10558, .F. ) ;
#6566 =( GEOMETRIC_REPRESENTATION_CONTEXT ( 3 ) GLOBAL_UNCERTAINTY_ASSIGNED_CONTEXT ( ( #9731 ) ) GLOBAL_UNIT_ASSIGNED_CONTEXT ( ( #7022, #2366, #8334 ) ) REPRESENTATION_CONTEXT ( 'NONE', 'WORKASPACE' ) );
#6567 = CARTESIAN_POINT ( 'NONE',  ( 2.733110507866247652, 28.87180007765647716, -3.862833514489153686 ) ) ;
#6568 = CARTESIAN_POINT ( 'NONE',  ( -5.279047395330986450E-15, -24.08636796417544446, -2.064782516116274280 ) ) ;
#6569 = ORIENTED_EDGE ( 'NONE', *, *, #5294, .T. ) ;
#6570 = CARTESIAN_POINT ( 'NONE',  ( -4.000000000000004441, -23.52818256558168031, -5.293929058800590504 ) ) ;
#6571 = CARTESIAN_POINT ( 'NONE',  ( 3.500000000000000444, 39.24680007765647360, -0.05647727720536935281 ) ) ;
#6572 = DIRECTION ( 'NONE',  ( 0.000000000000000000, 1.000000000000000000, 0.000000000000000000 ) ) ;
#6573 = AXIS2_PLACEMENT_3D ( 'NONE', #15449, #2745, #6716 ) ;
#6574 = CARTESIAN_POINT ( 'NONE',  ( 2.121784821874994176, -23.43695996064828435, -2.782732417011581028 ) ) ;
#6575 = AXIS2_PLACEMENT_3D ( 'NONE', #11492, #9837, #12712 ) ;
#6576 = CARTESIAN_POINT ( 'NONE',  ( 2.121784821875004390, -20.71777771588989125, -11.71380804911548701 ) ) ;
#6577 = CARTESIAN_POINT ( 'NONE',  ( 0.1370520045797951059, -30.29850743920613709, -11.99201766838188554 ) ) ;
#6578 = ORIENTED_EDGE ( 'NONE', *, *, #7259, .T. ) ;
#6579 = DIRECTION ( 'NONE',  ( -0.000000000000000000, 0.5000000000000002220, -0.8660254037844384856 ) ) ;
#6580 = AXIS2_PLACEMENT_3D ( 'NONE', #6772, #8348, #2443 ) ;
#6581 = CARTESIAN_POINT ( 'NONE',  ( 2.115076519116362963, 16.37180007765647716, -3.012182706137107591 ) ) ;
#6582 = CARTESIAN_POINT ( 'NONE',  ( -1.071796769724477238, -25.91398618305211343, -5.753740464163247914 ) ) ;
#6583 = CARTESIAN_POINT ( 'NONE',  ( 2.121784821874994176, -29.92195854414224598, -12.04427021775403084 ) ) ;
#6584 = VERTEX_POINT ( 'NONE', #9482 ) ;
#6585 = CARTESIAN_POINT ( 'NONE',  ( -2.115076519116425580, 32.37819992234354771, -3.012182706137062738 ) ) ;
#6586 = CARTESIAN_POINT ( 'NONE',  ( 2.864755990943222308, 15.50319992234354416, -2.011557305968548093 ) ) ;
#6587 = CARTESIAN_POINT ( 'NONE',  ( -2.121784821875005722, -23.47997819337460257, -2.844168820333258907 ) ) ;
#6588 = CARTESIAN_POINT ( 'NONE',  ( -0.05938372350926768989, 31.12180007765648426, -2.628655560595669183 ) ) ;
#6589 = ADVANCED_FACE ( 'NONE', ( #9757 ), #3740, .T. ) ;
#6590 = CIRCLE ( 'NONE', #11603, 2.200000000000000622 ) ;
#6591 = CARTESIAN_POINT ( 'NONE',  ( -1.336863392178569088, 22.50319992234354416, -4.297206761780648421 ) ) ;
#6592 = AXIS2_PLACEMENT_3D ( 'NONE', #15407, #9812, #15493 ) ;
#6593 = UNCERTAINTY_MEASURE_WITH_UNIT (LENGTH_MEASURE( 1.000000000000000082E-05 ), #16139, 'distance_accuracy_value', 'NONE');
#6594 = CARTESIAN_POINT ( 'NONE',  ( -2.000000000000005773, -28.06608030478504290, -9.761559716304219592 ) ) ;
#6595 = ORIENTED_EDGE ( 'NONE', *, *, #9977, .T. ) ;
#6596 = CARTESIAN_POINT ( 'NONE',  ( 4.730628863548789710E-15, -16.33737451245578498, -7.593689001224928958 ) ) ;
#6597 = CARTESIAN_POINT ( 'NONE',  ( 4.499999999999999112, 36.74680007765647360, -0.05647727720537982360 ) ) ;
#6598 = DIRECTION ( 'NONE',  ( 0.000000000000000000, 0.000000000000000000, -1.000000000000000000 ) ) ;
#6599 = CARTESIAN_POINT ( 'NONE',  ( -4.243569643750000786, -24.12611217186045565, -10.17417894125829037 ) ) ;
#6600 = LINE ( 'NONE', #3461, #10563 ) ;
#6601 = CIRCLE ( 'NONE', #4519, 0.9999999999999991118 ) ;
#6602 = CARTESIAN_POINT ( 'NONE',  ( 2.000000000000004441, -18.45466017170117112, -8.113982932514955948 ) ) ;
#6603=STYLED_ITEM('',(#18424),#2218);
#6604 = CARTESIAN_POINT ( 'NONE',  ( 2.000000000000004441, -19.74520715349101607, -9.957075032165194628 ) ) ;
#6605 = EDGE_LOOP ( 'NONE', ( #14810, #5838, #14288, #551, #17439, #8398 ) ) ;
#6606 = ORIENTED_EDGE ( 'NONE', *, *, #16591, .F. ) ;
#6607 =( BOUNDED_CURVE ( )  B_SPLINE_CURVE ( 2, ( #15913, #8656, #11817, #7364, #11629, #4680, #8569, #13120, #17323 ),
 .UNSPECIFIED., .F., .F. ) 
 B_SPLINE_CURVE_WITH_KNOTS ( ( 3, 2, 2, 2, 3 ),
 ( 0.6810344827586206629, 0.6839080459770114917, 0.6896551724137931494, 0.6954022988505746961, 0.6982758620689655249 ),
 .UNSPECIFIED. ) 
 CURVE ( )  GEOMETRIC_REPRESENTATION_ITEM ( )  RATIONAL_B_SPLINE_CURVE ( ( 0.9330127018922194093, 0.9330127018922194093, 1.000000000000000000, 0.8660254037844387076, 1.000000000000000000, 0.8660254037844387076, 1.000000000000000000, 0.9330127018922194093, 0.9330127018922194093 ) ) 
 REPRESENTATION_ITEM ( '' )  );
#6608 = DIRECTION ( 'NONE',  ( 0.000000000000000000, 0.000000000000000000, 1.000000000000000000 ) ) ;
#6609 = ADVANCED_FACE ( 'NONE', ( #15157 ), #12012, .T. ) ;
#6610 = ADVANCED_FACE ( 'NONE', ( #16742 ), #18318, .T. ) ;
#6611 = CARTESIAN_POINT ( 'NONE',  ( -1.734723475976807094E-15, 16.59999999999999787, -2.500000000000000000 ) ) ;
#6612 = CARTESIAN_POINT ( 'NONE',  ( 6.618852602794225604, -14.16203062248956712, -2.127031534456948147 ) ) ;
#6613 = VERTEX_POINT ( 'NONE', #8282 ) ;
#6614 = CARTESIAN_POINT ( 'NONE',  ( -2.798362969681409851, 14.75319992234354594, -2.102939460078765421 ) ) ;
#6615 = EDGE_CURVE ( 'NONE', #17585, #8977, #1249, .T. ) ;
#6616 = CARTESIAN_POINT ( 'NONE',  ( -2.121784821874996396, -20.64249580861881128, -11.60629434330255982 ) ) ;
#6617 = CARTESIAN_POINT ( 'NONE',  ( 2.864755990943265829, 29.49680007765647716, 2.011557305968487697 ) ) ;
#6618 = CARTESIAN_POINT ( 'NONE',  ( -2.798362969681409851, 19.75319992234354416, -2.102939460078765421 ) ) ;
#6619 = DIRECTION ( 'NONE',  ( -0.000000000000000000, 1.000000000000000000, -0.000000000000000000 ) ) ;
#6620 = CARTESIAN_POINT ( 'NONE',  ( 4.898587196589409870E-16, 4.000000000000007105, -4.000000000000000000 ) ) ;
#6621 = CONICAL_SURFACE ( 'NONE', #14624, 3.047499999999999876, 1.047197551196590748 ) ;
#6622 = CARTESIAN_POINT ( 'NONE',  ( -4.243569643750005227, -26.66002939159267271, -9.521497656227012385 ) ) ;
#6623 = CARTESIAN_POINT ( 'NONE',  ( 4.000000000000000000, -1.759474945355381292, 3.047500000000002540 ) ) ;
#6624 = CARTESIAN_POINT ( 'NONE',  ( -1.444289557196047014, 23.49680007765647716, -4.262301884875704161 ) ) ;
#6625 = CARTESIAN_POINT ( 'NONE',  ( 0.000000000000000000, 5.000000000000000000, 0.000000000000000000 ) ) ;
#6626 = CARTESIAN_POINT ( 'NONE',  ( 14.99999999999999822, 13.00000000000000178, 24.99999999999999645 ) ) ;
#6627 = CARTESIAN_POINT ( 'NONE',  ( 2.121784821875004390, -18.36252947412342351, -8.350164967253801862 ) ) ;
#6628 = VERTEX_POINT ( 'NONE', #15522 ) ;
#6629 = CARTESIAN_POINT ( 'NONE',  ( -14.99999999999999645, 10.00000000000000000, 30.00000000000000000 ) ) ;
#6630 = CARTESIAN_POINT ( 'NONE',  ( -9.000000000000001776, 38.59999999999999432, 2.499999999999998224 ) ) ;
#6631 = CARTESIAN_POINT ( 'NONE',  ( -2.500000000000001332, 14.50319992234354771, -0.05647727720530596601 ) ) ;
#6632 = CARTESIAN_POINT ( 'NONE',  ( 4.000000000000003553, -21.48691976548304439, -10.43133947375997472 ) ) ;
#6633 = CARTESIAN_POINT ( 'NONE',  ( -0.05938372350927861865, 31.12180007765647360, -3.680117784833935701 ) ) ;
#6634 = DIRECTION ( 'NONE',  ( -0.000000000000000000, 1.000000000000000000, -0.000000000000000000 ) ) ;
#6635 = CARTESIAN_POINT ( 'NONE',  ( -3.912726941231881472, 15.00000000000000178, -0.8267756552389129432 ) ) ;
#6636 = ORIENTED_EDGE ( 'NONE', *, *, #15742, .F. ) ;
#6637 = CARTESIAN_POINT ( 'NONE',  ( 4.243569643750003451, -19.16166480309071218, -7.355703438614951573 ) ) ;
#6638 = EDGE_CURVE ( 'NONE', #11926, #12347, #4199, .T. ) ;
#6639 = CARTESIAN_POINT ( 'NONE',  ( -2.115076519116362519, 22.62180007765647360, 3.012182706137107147 ) ) ;
#6640 = VERTEX_POINT ( 'NONE', #401 ) ;
#6641 = CARTESIAN_POINT ( 'NONE',  ( 4.730628863548789710E-15, -22.75784574686024797, -16.76307219698486506 ) ) ;
#6642 = CARTESIAN_POINT ( 'NONE',  ( 3.046716722576175318, -24.86286735169470319, -16.06997776478271334 ) ) ;
#6643 = CARTESIAN_POINT ( 'NONE',  ( 7.502920075503393349, -12.79035154381909756, 6.457010517113837444 ) ) ;
#6644 = CARTESIAN_POINT ( 'NONE',  ( -5.330712181944245322E-15, -30.65656652402004312, -10.95765408413266861 ) ) ;
#6645 = VERTEX_POINT ( 'NONE', #9847 ) ;
#6646 = DIRECTION ( 'NONE',  ( -4.915049848600951133E-16, 0.000000000000000000, -1.000000000000000000 ) ) ;
#6647 = CARTESIAN_POINT ( 'NONE',  ( 3.999999999999996447, -23.76478284628143811, -5.631829278076560641 ) ) ;
#6648 = CARTESIAN_POINT ( 'NONE',  ( -3.500000000000000444, 27.99680007765648071, 0.05647727720536892260 ) ) ;
#6649 = VERTEX_POINT ( 'NONE', #8447 ) ;
#6650 = ORIENTED_EDGE ( 'NONE', *, *, #4551, .F. ) ;
#6651 = CARTESIAN_POINT ( 'NONE',  ( -4.000000000000000888, -21.14172227611897270, -5.912028460313731415 ) ) ;
#6652 = EDGE_CURVE ( 'NONE', #1834, #14266, #15816, .T. ) ;
#6653 = APPLICATION_CONTEXT ( 'automotive_design' ) ;
#6654 = CARTESIAN_POINT ( 'NONE',  ( 1.444289557195957086, 32.75319992234354061, -4.262301884875733471 ) ) ;
#6655 = CARTESIAN_POINT ( 'NONE',  ( 1.533898589781675205E-14, -26.93489706776514581, -7.211752309227528634 ) ) ;
#6656 = CARTESIAN_POINT ( 'NONE',  ( -2.481649420246391902, 27.12819992234355126, -0.8687765177875723666 ) ) ;
#6657 = EDGE_CURVE ( 'NONE', #13482, #12581, #12608, .T. ) ;
#6658 = ORIENTED_EDGE ( 'NONE', *, *, #13615, .T. ) ;
#6659 = CARTESIAN_POINT ( 'NONE',  ( -0.05938372350928957516, 23.62180007765647005, -4.731580009072201776 ) ) ;
#6660 = CARTESIAN_POINT ( 'NONE',  ( 1.999999999999994449, -23.89331173033122369, -3.802228594101777492 ) ) ;
#6661 = ORIENTED_EDGE ( 'NONE', *, *, #17545, .T. ) ;
#6662 = CARTESIAN_POINT ( 'NONE',  ( -4.000000000000000888, -21.65794106883490855, -6.649265300173826887 ) ) ;
#6663 = CARTESIAN_POINT ( 'NONE',  ( -1.027846397803541700, 39.99680007765648071, 3.346150245485522312 ) ) ;
#6664 = CARTESIAN_POINT ( 'NONE',  ( -14.99999999999999645, -10.00000000000000000, -30.00000000000000000 ) ) ;
#6665 = CARTESIAN_POINT ( 'NONE',  ( -4.243569643750004339, -22.75612477167839387, -3.946144054785039934 ) ) ;
#6666 = CARTESIAN_POINT ( 'NONE',  ( 4.243569643750003451, -20.19410238852258743, -8.830177118335141628 ) ) ;
#6667 = CARTESIAN_POINT ( 'NONE',  ( 9.000000000000005329, 29.79999999999999716, 2.499999999999997335 ) ) ;
#6668 = ORIENTED_EDGE ( 'NONE', *, *, #15462, .F. ) ;
#6669 = CARTESIAN_POINT ( 'NONE',  ( 1.999999999999994449, -27.31326123277925433, -8.686422659181676664 ) ) ;
#6670 = DIRECTION ( 'NONE',  ( -3.469446951953613696E-16, -0.000000000000000000, -1.000000000000000000 ) ) ;
#6671 = DIRECTION ( 'NONE',  ( 0.000000000000000000, -0.5000000000000011102, -0.8660254037844380415 ) ) ;
#6672 = EDGE_LOOP ( 'NONE', ( #5574, #16692, #11138, #9423, #7931 ) ) ;
#6673 = CARTESIAN_POINT ( 'NONE',  ( -1.135272562821019626, 31.50319992234354416, 3.311245368580577164 ) ) ;
#6674 = CARTESIAN_POINT ( 'NONE',  ( 3.518350579753606322, 23.12819992234354416, -1.080741659609876892 ) ) ;
#6675 = ADVANCED_FACE ( 'NONE', ( #12811 ), #11236, .F. ) ;
#6676 = CARTESIAN_POINT ( 'NONE',  ( -5.330712181944245322E-15, -24.72005040778675777, -2.479430425741570243 ) ) ;
#6677 = CARTESIAN_POINT ( 'NONE',  ( 0.7188294034286049072, 26.24680007765647716, -2.395093729190366005 ) ) ;
#6678 = CARTESIAN_POINT ( 'NONE',  ( 3.607379964056363075, 23.50319992234354416, 2.690724712371229010 ) ) ;
#6679 = CARTESIAN_POINT ( 'NONE',  ( -1.999999999999996225, -22.21875553454993124, -13.48966822215472305 ) ) ;
#6680 = EDGE_LOOP ( 'NONE', ( #8978, #1993, #1506, #4040 ) ) ;
#6681 = CARTESIAN_POINT ( 'NONE',  ( 4.730628863548789710E-15, -16.07926511609781528, -7.225070581294880334 ) ) ;
#6682 = CARTESIAN_POINT ( 'NONE',  ( -0.05938372350928957516, 36.12180007765646650, -4.731580009072201776 ) ) ;
#6683 = AXIS2_PLACEMENT_3D ( 'NONE', #18221, #11051, #11226 ) ;
#6684 = CARTESIAN_POINT ( 'NONE',  ( -4.243569643749998122, -22.91500560846283463, -12.71602962843106432 ) ) ;
#6685 = CARTESIAN_POINT ( 'NONE',  ( -6.158835246850665095E-15, -22.83371997885389604, -15.30223878937131587 ) ) ;
#6686 = CYLINDRICAL_SURFACE ( 'NONE', #5042, 0.9999999999999991118 ) ;
#6687 = VERTEX_POINT ( 'NONE', #15880 ) ;
#6688 = ORIENTED_EDGE ( 'NONE', *, *, #909, .F. ) ;
#6689 = DIRECTION ( 'NONE',  ( 0.000000000000000000, 0.000000000000000000, -1.000000000000000000 ) ) ;
#6690 = DIRECTION ( 'NONE',  ( 0.000000000000000000, -1.000000000000000000, 0.000000000000000000 ) ) ;
#6691 = CARTESIAN_POINT ( 'NONE',  ( 4.000000000000003553, -19.68015399097727069, -7.851010534249639683 ) ) ;
#6692 = CARTESIAN_POINT ( 'NONE',  ( 1.071796769724495224, -22.58713728321475855, -14.95008220409718369 ) ) ;
#6693 = ORIENTED_EDGE ( 'NONE', *, *, #5181, .T. ) ;
#6694 = CARTESIAN_POINT ( 'NONE',  ( 0.7188294034286553114, 33.75319992234354771, 2.395093729190349130 ) ) ;
#6695 = CARTESIAN_POINT ( 'NONE',  ( -4.243569643750000786, -24.12611217186045565, -10.17417894125829037 ) ) ;
#6696 = CARTESIAN_POINT ( 'NONE',  ( -1.027846397803541700, 29.99680007765648071, 3.346150245485522312 ) ) ;
#6697 = CARTESIAN_POINT ( 'NONE',  ( 3.500000000000000444, 23.25319992234354416, 0.05647727720529520379 ) ) ;
#6698 = CARTESIAN_POINT ( 'NONE',  ( -10.00000000000000178, 40.79999999999999716, -2.500000000000001776 ) ) ;
#6699 = LINE ( 'NONE', #5223, #13495 ) ;
#6700 = CARTESIAN_POINT ( 'NONE',  ( -2.121784821874996396, -20.93286887952152497, -12.02099006572386486 ) ) ;
#6701 = EDGE_CURVE ( 'NONE', #2806, #9378, #13794, .T. ) ;
#6702 = EDGE_CURVE ( 'NONE', #12103, #2069, #4370, .T. ) ;
#6703 =( BOUNDED_CURVE ( )  B_SPLINE_CURVE ( 2, ( #14692, #17936, #13642, #9740, #5393, #5483, #14010, #15051, #10861 ),
 .UNSPECIFIED., .F., .F. ) 
 B_SPLINE_CURVE_WITH_KNOTS ( ( 3, 2, 2, 2, 3 ),
 ( 0.3706896551724138122, 0.3735632183908045856, 0.3793103448275861878, 0.3850574712643677899, 0.3879310344827586188 ),
 .UNSPECIFIED. ) 
 CURVE ( )  GEOMETRIC_REPRESENTATION_ITEM ( )  RATIONAL_B_SPLINE_CURVE ( ( 0.9330127018922194093, 0.9330127018922200755, 1.000000000000000000, 0.8660254037844387076, 1.000000000000000000, 0.8660254037844387076, 1.000000000000000000, 0.9330127018922194093, 0.9330127018922194093 ) ) 
 REPRESENTATION_ITEM ( '' )  );
#6704 = CARTESIAN_POINT ( 'NONE',  ( -1.734723475976807094E-15, 43.00000000000000000, -2.500000000000000000 ) ) ;
#6705 = CARTESIAN_POINT ( 'NONE',  ( 0.05938372350929014415, 22.37180007765647716, 4.731580009072201776 ) ) ;
#6706 = EDGE_CURVE ( 'NONE', #7005, #13964, #12991, .T. ) ;
#6707 = FACE_OUTER_BOUND ( 'NONE', #7650, .T. ) ;
#6708 = DIRECTION ( 'NONE',  ( 0.000000000000000000, -1.000000000000000000, 0.000000000000000000 ) ) ;
#6709 = AXIS2_PLACEMENT_3D ( 'NONE', #772, #2356, #9375 ) ;
#6710 = CARTESIAN_POINT ( 'NONE',  ( 4.243569643749996345, -24.47685408073152402, -6.403600187652020992 ) ) ;
#6711 = CARTESIAN_POINT ( 'NONE',  ( 1.071796769724494780, -28.02033530227262048, -8.761918760281082186 ) ) ;
#6712 = DIRECTION ( 'NONE',  ( 0.000000000000000000, 1.000000000000000000, 0.000000000000000000 ) ) ;
#6713 = ADVANCED_FACE ( 'NONE', ( #12724 ), #26, .T. ) ;
#6714 = CARTESIAN_POINT ( 'NONE',  ( 1.593127413382998903, 37.12180007765648071, 2.091722143975139669 ) ) ;
#6715 = DIRECTION ( 'NONE',  ( -0.000000000000000000, -1.000000000000000000, -0.000000000000000000 ) ) ;
#6716 = DIRECTION ( 'NONE',  ( 0.000000000000000000, -0.000000000000000000, 1.000000000000000000 ) ) ;
#6717 = CARTESIAN_POINT ( 'NONE',  ( -2.000000000000005773, -29.42115463636932304, -11.69680642194373554 ) ) ;
#6718 = DIRECTION ( 'NONE',  ( -0.000000000000000000, -1.000000000000000000, -0.000000000000000000 ) ) ;
#6719 = ADVANCED_FACE ( 'NONE', ( #10109 ), #11322, .T. ) ;
#6720 = EDGE_LOOP ( 'NONE', ( #1304, #11478, #13465 ) ) ;
#6721 = CARTESIAN_POINT ( 'NONE',  ( 2.121784821874994176, -23.72733303155099804, -3.197428139432884286 ) ) ;
#6722 = CARTESIAN_POINT ( 'NONE',  ( 3.518350579753631191, 21.87180007765647360, 1.080741659609802285 ) ) ;
#6723 = AXIS2_PLACEMENT_3D ( 'NONE', #12020, #6090, #10256 ) ;
#6724 = VERTEX_POINT ( 'NONE', #8719 ) ;
#6725 = PRODUCT_DEFINITION ( 'UNKNOWN', '', #3619, #936 ) ;
#6726 = CARTESIAN_POINT ( 'NONE',  ( -6.428571428571423496, -11.73421655796351892, 14.25837509840161310 ) ) ;
#6727 = FACE_BOUND ( 'NONE', #10459, .T. ) ;
#6728 = CARTESIAN_POINT ( 'NONE',  ( -3.877086799165925690, -27.97239129529922508, -13.72246263182690917 ) ) ;
#6729 = CARTESIAN_POINT ( 'NONE',  ( 1.999999999999994449, -29.31360905384856608, -11.54321541263277950 ) ) ;
#6730 = DIRECTION ( 'NONE',  ( -1.000000000000000000, 0.000000000000000000, 0.000000000000000000 ) ) ;
#6731 = CARTESIAN_POINT ( 'NONE',  ( 2.121784821874994176, -28.85725728416562674, -10.52371923554258260 ) ) ;
#6732 = ORIENTED_EDGE ( 'NONE', *, *, #4619, .T. ) ;
#6733 = CARTESIAN_POINT ( 'NONE',  ( -4.000000000000000888, -23.46470684334068935, -9.229594239684162815 ) ) ;
#6734 = CARTESIAN_POINT ( 'NONE',  ( -4.000000000000000888, -21.20624962591340790, -6.004183066303009575 ) ) ;
#6735 = AXIS2_PLACEMENT_3D ( 'NONE', #3424, #9400, #2474 ) ;
#6736 = CARTESIAN_POINT ( 'NONE',  ( -2.518350579753628526, 18.12180007765648071, -0.7558219633769075463 ) ) ;
#6737 = CONICAL_SURFACE ( 'NONE', #1722, 2.000000000000001776, 1.029744260000000189 ) ;
#6738 = VERTEX_POINT ( 'NONE', #11500 ) ;
#6739 = FACE_OUTER_BOUND ( 'NONE', #11852, .T. ) ;
#6740 = CARTESIAN_POINT ( 'NONE',  ( -4.499999999999999112, 32.00319992234354061, -0.05647727720528529505 ) ) ;
#6741 = UNCERTAINTY_MEASURE_WITH_UNIT (LENGTH_MEASURE( 1.000000000000000082E-05 ), #3895, 'distance_accuracy_value', 'NONE');
#6742 = CARTESIAN_POINT ( 'NONE',  ( -3.999999999999997335, -18.49715259029829539, -6.161509441896827255 ) ) ;
#6743 = CARTESIAN_POINT ( 'NONE',  ( -2.055738996568281518, 26.75319992234354771, 1.423772053676066962 ) ) ;
#6744 = VERTEX_POINT ( 'NONE', #17196 ) ;
#6745 = CARTESIAN_POINT ( 'NONE',  ( 2.121784821874994176, -28.11519276963646519, -9.463941278243694910 ) ) ;
#6746 = CARTESIAN_POINT ( 'NONE',  ( -4.481649420246366589, 25.37180007765648426, 1.518615910253458878 ) ) ;
#6747 = CARTESIAN_POINT ( 'NONE',  ( -3.999999999999997335, -19.27148077937220449, -7.267364701686970463 ) ) ;
#6748 = ORIENTED_EDGE ( 'NONE', *, *, #7500, .T. ) ;
#6749 = FACE_OUTER_BOUND ( 'NONE', #11199, .T. ) ;
#6750 = AXIS2_PLACEMENT_3D ( 'NONE', #11221, #14195, #1498 ) ;
#6751 = DIRECTION ( 'NONE',  ( 0.000000000000000000, -0.5000000000000000000, -0.8660254037844385966 ) ) ;
#6752 = DIRECTION ( 'NONE',  ( 0.000000000000000000, 0.000000000000000000, -1.000000000000000000 ) ) ;
#6753 = CARTESIAN_POINT ( 'NONE',  ( 4.243569643750000786, -22.48066477007841613, -7.824236514204232940 ) ) ;
#6754 = LINE ( 'NONE', #5373, #6436 ) ;
#6755 = ORIENTED_EDGE ( 'NONE', *, *, #12262, .T. ) ;
#6756 = CARTESIAN_POINT ( 'NONE',  ( -3.999999999999997335, -22.17521148910429574, -11.41432192690677283 ) ) ;
#6757 = DIRECTION ( 'NONE',  ( -0.000000000000000000, 1.000000000000000000, -0.000000000000000000 ) ) ;
#6758 = CARTESIAN_POINT ( 'NONE',  ( -14.99999999999999645, -10.00000000000000000, 30.00000000000000000 ) ) ;
#6759 = ORIENTED_EDGE ( 'NONE', *, *, #2858, .T. ) ;
#6760 = VECTOR ( 'NONE', #17489, 1000.000000000000000 ) ;
#6761 = CARTESIAN_POINT ( 'NONE',  ( -1.027846397803611866, 35.00319992234354771, -3.346150245485499219 ) ) ;
#6762 = CARTESIAN_POINT ( 'NONE',  ( 2.864755990943222308, 18.00319992234354771, -2.011557305968548093 ) ) ;
#6763 = VECTOR ( 'NONE', #13070, 1000.000000000000000 ) ;
#6764 = CARTESIAN_POINT ( 'NONE',  ( 3.250767337421092140, -21.87258502241503066, -2.200193550433863887 ) ) ;
#6765 = CARTESIAN_POINT ( 'NONE',  ( -1.593127413382998459, 33.37180007765648071, -2.091722143975139669 ) ) ;
#6766 = CARTESIAN_POINT ( 'NONE',  ( 2.733110507866328920, 28.62819992234354416, 3.862833514489095510 ) ) ;
#6767 = CARTESIAN_POINT ( 'NONE',  ( -4.000000000000000888, -24.75525382513053430, -11.07268633933439972 ) ) ;
#6768 = ORIENTED_EDGE ( 'NONE', *, *, #5542, .T. ) ;
#6769 = ADVANCED_FACE ( 'NONE', ( #1794 ), #10001, .T. ) ;
#6770 = CARTESIAN_POINT ( 'NONE',  ( -4.243569643750000786, -20.54484429739364515, -5.059598364728879361 ) ) ;
#6771 = CARTESIAN_POINT ( 'NONE',  ( -2.798362969681365886, 20.24680007765647716, 2.102939460078824929 ) ) ;
#6772 = CARTESIAN_POINT ( 'NONE',  ( -9.000000000000001776, 27.59999999999999432, 2.499999999999995559 ) ) ;
#6773 = VECTOR ( 'NONE', #6843, 1000.000000000000000 ) ;
#6774 = CARTESIAN_POINT ( 'NONE',  ( 2.121784821874994176, -26.79238211330187625, -7.574771876102201595 ) ) ;
#6775 = EDGE_CURVE ( 'NONE', #16719, #8888, #13921, .T. ) ;
#6776 = DIRECTION ( 'NONE',  ( 1.000000000000000000, 0.000000000000000000, 0.000000000000000000 ) ) ;
#6777 = DIRECTION ( 'NONE',  ( 0.000000000000000000, -1.000000000000000000, 0.000000000000000000 ) ) ;
#6778 = EDGE_CURVE ( 'NONE', #2439, #8594, #12174, .T. ) ;
#6779 = DIRECTION ( 'NONE',  ( -0.000000000000000000, -1.000000000000000000, -0.000000000000000000 ) ) ;
#6780 = EDGE_LOOP ( 'NONE', ( #17606, #3611, #189, #9160 ) ) ;
#6781 = ORIENTED_EDGE ( 'NONE', *, *, #17289, .F. ) ;
#6782 = CARTESIAN_POINT ( 'NONE',  ( -3.518350579753630747, 18.12180007765648071, -1.080741659609802729 ) ) ;
#6783 = DIRECTION ( 'NONE',  ( 0.000000000000000000, 0.000000000000000000, -1.000000000000000000 ) ) ;
#6784 = CIRCLE ( 'NONE', #10637, 0.9999999999999991118 ) ;
#6785 = FACE_OUTER_BOUND ( 'NONE', #11797, .T. ) ;
#6786 = CARTESIAN_POINT ( 'NONE',  ( 4.000000000000003553, -20.97070097276711209, -9.694102633899875698 ) ) ;
#6787 = VERTEX_POINT ( 'NONE', #8344 ) ;
#6788 = CARTESIAN_POINT ( 'NONE',  ( 2.481649420246391902, 35.87819992234354771, 0.8687765177875720335 ) ) ;
#6789 = VECTOR ( 'NONE', #16843, 1000.000000000000000 ) ;
#6790 = CARTESIAN_POINT ( 'NONE',  ( 4.243569643750003451, -22.22671388484159039, -11.73304717528426977 ) ) ;
#6791 = CARTESIAN_POINT ( 'NONE',  ( 3.500000000000000444, 29.24680007765647716, -0.05647727720536935281 ) ) ;
#6792 = PRODUCT ( 'socket head cap screw_iso_ISO 4762 M8 x 12 - 12N', 'socket head cap screw_iso_ISO 4762 M8 x 12 - 12N', '', ( #14937 ) ) ;
#6793 = CIRCLE ( 'NONE', #15416, 1.899999999999999689 ) ;
#6794 = CARTESIAN_POINT ( 'NONE',  ( -2.798362969681409851, 29.75319992234354416, -2.102939460078765421 ) ) ;
#6795 = CARTESIAN_POINT ( 'NONE',  ( 14.20000000000000107, 0.000000000000000000, 0.000000000000000000 ) ) ;
#6796 = AXIS2_PLACEMENT_3D ( 'NONE', #11100, #12222, #7957 ) ;
#6797 = DIRECTION ( 'NONE',  ( 1.000000000000000000, 0.000000000000000000, 0.000000000000000000 ) ) ;
#6798 = CARTESIAN_POINT ( 'NONE',  ( 4.730628863548789710E-15, -20.46712485418328242, -13.49158372010569273 ) ) ;
#6799 = EDGE_CURVE ( 'NONE', #4066, #8485, #11905, .T. ) ;
#6800 = DIRECTION ( 'NONE',  ( -3.469446951953613696E-16, -0.000000000000000000, -1.000000000000000000 ) ) ;
#6801 = AXIS2_PLACEMENT_3D ( 'NONE', #13853, #15442, #4021 ) ;
#6802 = CYLINDRICAL_SURFACE ( 'NONE', #18084, 4.000000000000000000 ) ;
#6803 = FACE_OUTER_BOUND ( 'NONE', #4150, .T. ) ;
#6804 = CARTESIAN_POINT ( 'NONE',  ( 4.243569643750000786, -22.19029169917569888, -7.409540791782929681 ) ) ;
#6805 = DIRECTION ( 'NONE',  ( 0.000000000000000000, 0.8191520442889952403, -0.5735764363510413855 ) ) ;
#6806 = DIRECTION ( 'NONE',  ( -6.162975822039154730E-33, 0.5735764363510414965, 0.8191520442889950182 ) ) ;
#6807 = CARTESIAN_POINT ( 'NONE',  ( -1.989345975306457071, 14.75319992234354771, -1.515154207786300944 ) ) ;
#6808 = DIRECTION ( 'NONE',  ( -3.469446951953613696E-16, -0.000000000000000000, -1.000000000000000000 ) ) ;
#6809 = CARTESIAN_POINT ( 'NONE',  ( 3.481649420246370141, 36.62180007765648071, -1.193696214020541602 ) ) ;
#6810 = CARTESIAN_POINT ( 'NONE',  ( 9.000000000000001776, 34.19999999999999574, -2.500000000000002665 ) ) ;
#6811 = EDGE_CURVE ( 'NONE', #5122, #4416, #12334, .T. ) ;
#6812 = ITEM_DEFINED_TRANSFORMATION ( 'NONE', 'NONE', #11020,  #16940 ) ;
#6813 = DIRECTION ( 'NONE',  ( -0.000000000000000000, -1.000000000000000000, -0.000000000000000000 ) ) ;
#6814 = ORIENTED_EDGE ( 'NONE', *, *, #9269, .F. ) ;
#6815 = CARTESIAN_POINT ( 'NONE',  ( -4.243569643750004339, -23.04649784258110756, -4.360839777206344081 ) ) ;
#6816 = CARTESIAN_POINT ( 'NONE',  ( -2.211161402132902243, 25.87180007765647360, -2.942372952327172886 ) ) ;
#6817 =( BOUNDED_CURVE ( )  B_SPLINE_CURVE ( 2, ( #3777, #2407, #9518, #13883, #12395, #13604, #15104, #2678, #8039 ),
 .UNSPECIFIED., .F., .T. ) 
 B_SPLINE_CURVE_WITH_KNOTS ( ( 3, 2, 2, 2, 3 ),
 ( 0.6120689655172414367, 0.6149425287356321546, 0.6206896551724138122, 0.6264367816091953589, 0.6293103448275861878 ),
 .UNSPECIFIED. ) 
 CURVE ( )  GEOMETRIC_REPRESENTATION_ITEM ( )  RATIONAL_B_SPLINE_CURVE ( ( 0.9330127018922194093, 0.9330127018922206306, 1.000000000000000000, 0.8660254037844387076, 1.000000000000000000, 0.8660254037844387076, 1.000000000000000000, 0.9330127018922194093, 0.9330127018922194093 ) ) 
 REPRESENTATION_ITEM ( '' )  );
#6818 = DIRECTION ( 'NONE',  ( -0.000000000000000000, -0.5735764363510414965, -0.8191520442889950182 ) ) ;
#6819 = CARTESIAN_POINT ( 'NONE',  ( 4.243569643750003451, -24.80780784842128028, -15.41923137458474535 ) ) ;
#6820 = DIRECTION ( 'NONE',  ( -0.000000000000000000, 1.000000000000000000, -0.000000000000000000 ) ) ;
#6821 = CARTESIAN_POINT ( 'NONE',  ( 4.898587196589413815E-16, 2.700915433685006750, 35.11257424290206330 ) ) ;
#6822 = DIRECTION ( 'NONE',  ( -1.000000000000000000, 0.000000000000000000, 4.336808689942021680E-16 ) ) ;
#6823 = CARTESIAN_POINT ( 'NONE',  ( -2.121784821875005722, -29.67460370596585406, -11.69101089865440457 ) ) ;
#6824 = ORIENTED_EDGE ( 'NONE', *, *, #15188, .F. ) ;
#6825 = CARTESIAN_POINT ( 'NONE',  ( 0.000000000000000000, 5.000000000000000000, 0.000000000000000000 ) ) ;
#6826 = CARTESIAN_POINT ( 'NONE',  ( 4.000000000000003553, -19.93826338733523684, -8.219628954179688307 ) ) ;
#6827 = AXIS2_PLACEMENT_3D ( 'NONE', #5164, #10818, #16493 ) ;
#6828 = CARTESIAN_POINT ( 'NONE',  ( 3.518350579753631191, 36.87180007765645939, 1.080741659609802285 ) ) ;
#6829 = ORIENTED_EDGE ( 'NONE', *, *, #337, .F. ) ;
#6830 = CARTESIAN_POINT ( 'NONE',  ( -6.158835246850665095E-15, -22.12391913957442213, -14.28853813557044639 ) ) ;
#6831 = EDGE_CURVE ( 'NONE', #13588, #17004, #9821, .T. ) ;
#6832 = CARTESIAN_POINT ( 'NONE',  ( 4.499999999999999112, 33.25319992234354771, 0.05647727720528474687 ) ) ;
#6833 = CARTESIAN_POINT ( 'NONE',  ( -1.071796769724486786, -17.14378655825974818, -7.176171716254351018 ) ) ;
#6834 = EDGE_CURVE ( 'NONE', #15647, #8512, #17133, .T. ) ;
#6835 = CARTESIAN_POINT ( 'NONE',  ( -2.500000000000001332, 27.00319992234355126, -0.05647727720530596601 ) ) ;
#6836 = VERTEX_POINT ( 'NONE', #9910 ) ;
#6837 = CARTESIAN_POINT ( 'NONE',  ( 2.121784821874994176, -28.63141156235240459, -10.20117811810379216 ) ) ;
#6838 = CARTESIAN_POINT ( 'NONE',  ( 2.829195390882805583, 24.62180007765647716, 3.793023760679204770 ) ) ;
#6839 = CARTESIAN_POINT ( 'NONE',  ( -5.279047395330986450E-15, -25.11880554960731970, -3.539256195836466112 ) ) ;
#6840 = ORIENTED_EDGE ( 'NONE', *, *, #18289, .F. ) ;
#6841 = PRESENTATION_LAYER_ASSIGNMENT (  '', '', ( #7725 ) ) ;
#6842 = CARTESIAN_POINT ( 'NONE',  ( 0.000000000000000000, -13.00000000000000178, -12.59063537424807677 ) ) ;
#6843 = DIRECTION ( 'NONE',  ( 0.000000000000000000, -0.5735764363510413855, -0.8191520442889951292 ) ) ;
#6844 = DIRECTION ( 'NONE',  ( -1.000000000000000000, 0.000000000000000000, 4.336808689942021680E-16 ) ) ;
#6845 = CARTESIAN_POINT ( 'NONE',  ( 14.20000000000000107, 0.000000000000000000, 0.000000000000000000 ) ) ;
#6846 = CARTESIAN_POINT ( 'NONE',  ( -2.121784821874996396, -19.38421250137371388, -9.809279546143578443 ) ) ;
#6847 = EDGE_LOOP ( 'NONE', ( #9333, #4524, #12672, #13933 ) ) ;
#6848 = DIRECTION ( 'NONE',  ( -1.000000000000000000, 0.000000000000000000, 0.000000000000000000 ) ) ;
#6849 = ORIENTED_EDGE ( 'NONE', *, *, #9077, .T. ) ;
#6850 = CARTESIAN_POINT ( 'NONE',  ( -1.999999999999996225, -21.25084529891249119, -12.10734914842380761 ) ) ;
#6851 = CARTESIAN_POINT ( 'NONE',  ( 9.000000000000000000, 20.99999999999999289, -2.500000000000001332 ) ) ;
#6852 = CARTESIAN_POINT ( 'NONE',  ( 9.000000000000005329, 31.99999999999999289, 2.499999999999997335 ) ) ;
#6853 = CARTESIAN_POINT ( 'NONE',  ( -1.071796769724486786, -22.56408388177708702, -14.91715853478535436 ) ) ;
#6854 = VERTEX_POINT ( 'NONE', #15504 ) ;
#6855 = CARTESIAN_POINT ( 'NONE',  ( -3.481649420246394122, 32.12819992234353350, -1.193696214020467883 ) ) ;
#6856 = CARTESIAN_POINT ( 'NONE',  ( -3.481649420246394566, 22.12819992234354061, -1.193696214020467883 ) ) ;
#6857 = CARTESIAN_POINT ( 'NONE',  ( 2.121784821875004390, -16.81387309597561242, -6.138454447673516334 ) ) ;
#6858 = CARTESIAN_POINT ( 'NONE',  ( 1.497042530366477164, 26.37180007765647716, -2.161531897785062384 ) ) ;
#6859 = CARTESIAN_POINT ( 'NONE',  ( -4.518350579753602325, 24.37819992234354416, 1.405661355842794391 ) ) ;
#6860 = CARTESIAN_POINT ( 'NONE',  ( -4.000000000000004441, -26.10927652916136310, -8.980113258101068752 ) ) ;
#6861 = EDGE_LOOP ( 'NONE', ( #11132, #387, #9553, #17347 ) ) ;
#6862 = AXIS2_PLACEMENT_3D ( 'NONE', #8595, #8780, #12956 ) ;
#6863 = CARTESIAN_POINT ( 'NONE',  ( -4.243569643750000786, -20.28673490103567545, -4.690979944798832513 ) ) ;
#6864 = CARTESIAN_POINT ( 'NONE',  ( -1.027846397803541700, 19.99680007765648071, 3.346150245485522312 ) ) ;
#6865 = CARTESIAN_POINT ( 'NONE',  ( -1.999999999999996225, -21.50895469527046444, -12.47596756835385534 ) ) ;
#6866 = CARTESIAN_POINT ( 'NONE',  ( 2.121784821874994176, -25.75994452787000100, -6.100298196382009763 ) ) ;
#6867 = CARTESIAN_POINT ( 'NONE',  ( 3.999999999999995559, 2.343145750507625191, -2.343145750507618086 ) ) ;
#6868 = FACE_OUTER_BOUND ( 'NONE', #7471, .T. ) ;
#6869 = ORIENTED_EDGE ( 'NONE', *, *, #12152, .F. ) ;
#6870 = ORIENTED_EDGE ( 'NONE', *, *, #14627, .T. ) ;
#6871 = DIRECTION ( 'NONE',  ( -3.469446951953613696E-16, -0.000000000000000000, -1.000000000000000000 ) ) ;
#6872 = CARTESIAN_POINT ( 'NONE',  ( 8.399999999999998579, 0.000000000000000000, 0.000000000000000000 ) ) ;
#6873 = AXIS2_PLACEMENT_3D ( 'NONE', #17329, #17420, #10619 ) ;
#6874 = CARTESIAN_POINT ( 'NONE',  ( -2.465190328815646976E-33, -26.97786251599082519, -14.24690051095425858 ) ) ;
#6875 = VERTEX_POINT ( 'NONE', #7035 ) ;
#6876 = TOROIDAL_SURFACE ( 'NONE', #13694, 9.000000000000003553, 0.9999999999999991118 ) ;
#6877 = CARTESIAN_POINT ( 'NONE',  ( -1.989345975306457071, 37.25319992234354061, -1.515154207786300944 ) ) ;
#6878 = CARTESIAN_POINT ( 'NONE',  ( 4.243569643750000786, -24.77138566275538523, -11.09572499108340793 ) ) ;
#6879 = CARTESIAN_POINT ( 'NONE',  ( 1.135272562821090458, 34.74680007765648071, 3.311245368580554072 ) ) ;
#6880 = EDGE_CURVE ( 'NONE', #6012, #5909, #13849, .T. ) ;
#6881 = CARTESIAN_POINT ( 'NONE',  ( -1.135272562821019626, 29.00319992234354416, 3.311245368580577164 ) ) ;
#6882 = EDGE_CURVE ( 'NONE', #18179, #16392, #1774, .T. ) ;
#6883 = DIRECTION ( 'NONE',  ( 0.000000000000000000, 0.000000000000000000, -1.000000000000000000 ) ) ;
#6884 = CARTESIAN_POINT ( 'NONE',  ( 4.243569643750000786, -23.51310235551028782, -9.298710193924424772 ) ) ;
#6885 = CIRCLE ( 'NONE', #17280, 8.000000000000001776 ) ;
#6886 = AXIS2_PLACEMENT_3D ( 'NONE', #11562, #4713, #5916 ) ;
#6887 = CARTESIAN_POINT ( 'NONE',  ( -1.281796014810987483, -15.42359483004433507, -10.64137488400932696 ) ) ;
#6888 =( REPRESENTATION_RELATIONSHIP ('NONE','NONE', #15868, #8990 ) REPRESENTATION_RELATIONSHIP_WITH_TRANSFORMATION ( #897 )SHAPE_REPRESENTATION_RELATIONSHIP( ) );
#6889 = CARTESIAN_POINT ( 'NONE',  ( -1.734723475976807094E-15, 40.79999999999999716, -2.500000000000000000 ) ) ;
#6890 = DIRECTION ( 'NONE',  ( 0.000000000000000000, 0.000000000000000000, -1.000000000000000000 ) ) ;
#6891 = CARTESIAN_POINT ( 'NONE',  ( -4.243569643750000786, -22.57745579371264455, -7.962468421678005726 ) ) ;
#6892 = DIRECTION ( 'NONE',  ( 0.000000000000000000, 1.000000000000000000, 0.000000000000000000 ) ) ;
#6893 = CARTESIAN_POINT ( 'NONE',  ( 2.481649420246374138, 36.62180007765647360, -0.8687765177876252132 ) ) ;
#6894 = CARTESIAN_POINT ( 'NONE',  ( 0.000000000000000000, 5.977523610840987267, 32.81826849749789687 ) ) ;
#6895 = CARTESIAN_POINT ( 'NONE',  ( -3.481649420246370141, 40.37180007765648071, 1.193696214020542268 ) ) ;
#6896 = EDGE_CURVE ( 'NONE', #11760, #7786, #4393, .T. ) ;
#6897 = CARTESIAN_POINT ( 'NONE',  ( -1.734723475976807094E-15, 34.19999999999999574, -2.500000000000000000 ) ) ;
#6898 = AXIS2_PLACEMENT_3D ( 'NONE', #12371, #5428, #9500 ) ;
#6899 = CIRCLE ( 'NONE', #11620, 8.000000000000001776 ) ;
#6900 = CARTESIAN_POINT ( 'NONE',  ( -1.055605843668875110, 15.00000000000000888, -3.337496964141338562 ) ) ;
#6901 = EDGE_CURVE ( 'NONE', #17767, #6613, #4090, .T. ) ;
#6902 = ORIENTED_EDGE ( 'NONE', *, *, #3163, .F. ) ;
#6903 = CARTESIAN_POINT ( 'NONE',  ( 4.243569643750000786, -21.44822718464654088, -6.349762834484042884 ) ) ;
#6904 = CARTESIAN_POINT ( 'NONE',  ( -2.798362969681365886, 32.74680007765648071, 2.102939460078824929 ) ) ;
#6905 = DIRECTION ( 'NONE',  ( -3.373073425510457965E-16, 0.000000000000000000, -1.000000000000000000 ) ) ;
#6906 = CARTESIAN_POINT ( 'NONE',  ( -8.500000000000005329, 0.000000000000000000, 18.49999999999999645 ) ) ;
#6907 = CYLINDRICAL_SURFACE ( 'NONE', #14405, 0.9999999999999991118 ) ;
#6908 = AXIS2_PLACEMENT_3D ( 'NONE', #7817, #3388, #11802 ) ;
#6909 = DIRECTION ( 'NONE',  ( -3.469446951953613696E-16, -0.000000000000000000, -1.000000000000000000 ) ) ;
#6910 = LINE ( 'NONE', #18346, #9392 ) ;
#6911 = CARTESIAN_POINT ( 'NONE',  ( -2.121784821874996396, -22.44926158312459208, -14.18662328281289398 ) ) ;
#6912 = ORIENTED_EDGE ( 'NONE', *, *, #7203, .F. ) ;
#6913 = CARTESIAN_POINT ( 'NONE',  ( -1.071796769724477238, -26.68831437212602609, -6.859595723953392010 ) ) ;
#6914 = CARTESIAN_POINT ( 'NONE',  ( 4.000000000000000888, -22.36774190952427688, -7.662965955988220834 ) ) ;
#6915 = CARTESIAN_POINT ( 'NONE',  ( 2.211161402132902243, 37.12180007765645939, 2.942372952327172442 ) ) ;
#6916 = PRODUCT_DEFINITION_CONTEXT ( 'detailed design', #5108, 'design' ) ;
#6917 = ORIENTED_EDGE ( 'NONE', *, *, #8304, .T. ) ;
#6918 = CARTESIAN_POINT ( 'NONE',  ( 1.071796769724485232, -28.79466349134653669, -9.867774020071223617 ) ) ;
#6919 = CARTESIAN_POINT ( 'NONE',  ( -1.444289557195956863, 39.00319992234354061, 4.262301884875733471 ) ) ;
#6920 = DIRECTION ( 'NONE',  ( 0.000000000000000000, 0.000000000000000000, 1.000000000000000000 ) ) ;
#6921 = CARTESIAN_POINT ( 'NONE',  ( -1.989345975306457071, 34.75319992234354771, -1.515154207786300944 ) ) ;
#6922 =( BOUNDED_CURVE ( )  B_SPLINE_CURVE ( 2, ( #5053, #3941, #5425, #17968, #9677, #4030, #13862, #15359, #16385 ),
 .UNSPECIFIED., .F., .T. ) 
 B_SPLINE_CURVE_WITH_KNOTS ( ( 3, 2, 2, 2, 3 ),
 ( 0.2500000000000000000, 0.2528735632183908288, 0.2586206896551724310, 0.2643678160919540332, 0.2672413793103448620 ),
 .UNSPECIFIED. ) 
 CURVE ( )  GEOMETRIC_REPRESENTATION_ITEM ( )  RATIONAL_B_SPLINE_CURVE ( ( 0.9330127018922194093, 0.9330127018922190762, 1.000000000000000000, 0.8660254037844387076, 1.000000000000000000, 0.8660254037844387076, 1.000000000000000000, 0.9330127018922187432, 0.9330127018922194093 ) ) 
 REPRESENTATION_ITEM ( '' )  );
#6923 = ORIENTED_EDGE ( 'NONE', *, *, #17154, .F. ) ;
#6924 = CARTESIAN_POINT ( 'NONE',  ( 2.121784821874994176, -29.14763035506834044, -10.93841495796388763 ) ) ;
#6925 = CARTESIAN_POINT ( 'NONE',  ( -4.518350579753632523, 23.12180007765647005, -1.405661355842698468 ) ) ;
#6926 = ORIENTED_EDGE ( 'NONE', *, *, #14043, .F. ) ;
#6927 =( LENGTH_UNIT ( ) NAMED_UNIT ( * ) SI_UNIT ( .MILLI., .METRE. ) );
#6928 = EDGE_CURVE ( 'NONE', #16586, #1458, #15702, .T. ) ;
#6929 = CARTESIAN_POINT ( 'NONE',  ( -5.577813053751546416E-15, -26.16056887869124381, -6.105897049437384538 ) ) ;
#6930 = DIRECTION ( 'NONE',  ( 0.000000000000000000, 0.000000000000000000, 1.000000000000000000 ) ) ;
#6931 = ADVANCED_FACE ( 'NONE', ( #1405 ), #15764, .F. ) ;
#6932 = CARTESIAN_POINT ( 'NONE',  ( -5.330712181944245322E-15, -26.30097046047931997, -4.737218247813111738 ) ) ;
#6933 = ORIENTED_EDGE ( 'NONE', *, *, #13615, .F. ) ;
#6934 = EDGE_CURVE ( 'NONE', #13129, #1761, #243, .T. ) ;
#6935 = DIRECTION ( 'NONE',  ( 0.000000000000000000, 0.000000000000000000, 1.000000000000000000 ) ) ;
#6936 = ORIENTED_EDGE ( 'NONE', *, *, #8689, .F. ) ;
#6937 = CARTESIAN_POINT ( 'NONE',  ( 4.713407268011036227E-15, -21.10080729779459574, -13.90623162973098559 ) ) ;
#6938 = DIRECTION ( 'NONE',  ( 0.000000000000000000, 0.8191520442889952403, -0.5735764363510413855 ) ) ;
#6939 = DIRECTION ( 'NONE',  ( -0.000000000000000000, -1.000000000000000000, -0.000000000000000000 ) ) ;
#6940 = APPLICATION_PROTOCOL_DEFINITION ( 'draft international standard', 'automotive_design', 1998, #7236 ) ;
#6941 = EDGE_CURVE ( 'NONE', #5271, #16039, #4178, .T. ) ;
#6942 = CARTESIAN_POINT ( 'NONE',  ( 3.673772985318163098, 15.50319992234354416, -2.599342558261029001 ) ) ;
#6943 = CARTESIAN_POINT ( 'NONE',  ( 2.864755990943222308, 23.00319992234354416, -2.011557305968548093 ) ) ;
#6944 = CARTESIAN_POINT ( 'NONE',  ( 2.000000000000004441, -23.87495749521851351, -15.85496975104595840 ) ) ;
#6945 = CARTESIAN_POINT ( 'NONE',  ( -1.989345975306426206, 30.24680007765648426, 1.515154207786343799 ) ) ;
#6946 = CARTESIAN_POINT ( 'NONE',  ( 4.481649420246397675, 25.87819992234355126, 1.518615910253363177 ) ) ;
#6947 = UNCERTAINTY_MEASURE_WITH_UNIT (LENGTH_MEASURE( 1.000000000000000082E-05 ), #10172, 'distance_accuracy_value', 'NONE');
#6948 = CARTESIAN_POINT ( 'NONE',  ( 1.999999999999994449, -26.99062448662684943, -8.225649633262349880 ) ) ;
#6949 = ORIENTED_EDGE ( 'NONE', *, *, #14842, .T. ) ;
#6950 = CARTESIAN_POINT ( 'NONE',  ( 4.243569643749996345, -22.18613318805455847, -3.132111710772846891 ) ) ;
#6951 = CARTESIAN_POINT ( 'NONE',  ( 2.798362969681366330, 23.99680007765647716, -2.102939460078824929 ) ) ;
#6952 = CARTESIAN_POINT ( 'NONE',  ( -5.577813053751546416E-15, -23.12778347219005681, -1.774630616266089866 ) ) ;
#6953 = PRODUCT_RELATED_PRODUCT_CATEGORY ( 'part', '', ( #6486 ) ) ;
#6954 = CARTESIAN_POINT ( 'NONE',  ( 4.243569643749997233, -24.21874468437355432, -6.034981767721972368 ) ) ;
#6955 = DIRECTION ( 'NONE',  ( 0.000000000000000000, -0.4999999999999992784, 0.8660254037844389297 ) ) ;
#6956 = DIRECTION ( 'NONE',  ( 0.000000000000000000, 0.000000000000000000, -1.000000000000000000 ) ) ;
#6957 = ORIENTED_EDGE ( 'NONE', *, *, #11270, .F. ) ;
#6958 = ORIENTED_EDGE ( 'NONE', *, *, #2424, .F. ) ;
#6959 = CARTESIAN_POINT ( 'NONE',  ( -3.500000000000000444, 20.49680007765647716, 0.05647727720536892260 ) ) ;
#6960 = CARTESIAN_POINT ( 'NONE',  ( -1.999999999999996225, -19.12144277825430549, -9.066247182994150222 ) ) ;
#6961 = FILL_AREA_STYLE_COLOUR ( '', #5996 ) ;
#6962 = CARTESIAN_POINT ( 'NONE',  ( -4.000000000000000888, -21.46435902227137760, -6.372801486233056423 ) ) ;
#6963 = CARTESIAN_POINT ( 'NONE',  ( 8.499999999999992895, 14.80000000000000071, 20.49999999999999645 ) ) ;
#6964 = ORIENTED_EDGE ( 'NONE', *, *, #15676, .T. ) ;
#6965 = CARTESIAN_POINT ( 'NONE',  ( -1.593127413382952939, 34.12819992234354771, 2.091722143975172532 ) ) ;
#6966 = CARTESIAN_POINT ( 'NONE',  ( 4.243569643750000786, -22.44840109553366858, -7.778159211712977417 ) ) ;
#6967 = CARTESIAN_POINT ( 'NONE',  ( -3.500000000000000444, 27.99680007765648071, 0.05647727720536892260 ) ) ;
#6968 = CARTESIAN_POINT ( 'NONE',  ( 3.500000000000000444, 30.75319992234354416, 0.05647727720529520379 ) ) ;
#6969 = CARTESIAN_POINT ( 'NONE',  ( 0.000000000000000000, -10.00000000000000178, -12.59063537424807677 ) ) ;
#6970 = CARTESIAN_POINT ( 'NONE',  ( 0.000000000000000000, 5.977523610840987267, 32.81826849749789687 ) ) ;
#6971 = CARTESIAN_POINT ( 'NONE',  ( -4.243569643750000786, -24.41648524276317289, -10.58887466367959540 ) ) ;
#6972 = DIRECTION ( 'NONE',  ( -0.000000000000000000, 1.000000000000000000, -0.000000000000000000 ) ) ;
#6973 = DIRECTION ( 'NONE',  ( 0.000000000000000000, 0.000000000000000000, -1.000000000000000000 ) ) ;
#6974 = CARTESIAN_POINT ( 'NONE',  ( -4.243569643750000786, -21.02879941556483345, -5.750757902097718421 ) ) ;
#6975 = CIRCLE ( 'NONE', #4912, 2.499999999999999556 ) ;
#6976 = CARTESIAN_POINT ( 'NONE',  ( -2.937035047792128761, 15.00000000000010125, -0.6671309589350113978 ) ) ;
#6977 = DIRECTION ( 'NONE',  ( -0.000000000000000000, -1.000000000000000000, -0.000000000000000000 ) ) ;
#6978 = EDGE_LOOP ( 'NONE', ( #9490, #3127, #16119 ) ) ;
#6979 = CARTESIAN_POINT ( 'NONE',  ( 1.989345975306457071, 16.00319992234354771, 1.515154207786300500 ) ) ;
#6980 = AXIS2_PLACEMENT_3D ( 'NONE', #10447, #16125, #3415 ) ;
#6981 = CARTESIAN_POINT ( 'NONE',  ( -2.121784821875005722, -29.41649430960788081, -11.32239247872435506 ) ) ;
#6982 = CARTESIAN_POINT ( 'NONE',  ( 3.518350579753631191, 34.37180007765648071, 1.080741659609802729 ) ) ;
#6983 = CARTESIAN_POINT ( 'NONE',  ( -9.891620614305184134, -9.933529378329316373, 2.554464806243397224 ) ) ;
#6984 = EDGE_LOOP ( 'NONE', ( #18039, #14574, #13989, #15198 ) ) ;
#6985 = CARTESIAN_POINT ( 'NONE',  ( -5.330712181944246111E-15, -25.26853287504744472, -3.262744568092922570 ) ) ;
#6986 = CARTESIAN_POINT ( 'NONE',  ( 1.027846397803542144, 33.74680007765648071, -3.346150245485522312 ) ) ;
#6987 = APPLICATION_CONTEXT ( 'automotive_design' ) ;
#6988 = SURFACE_SIDE_STYLE ('',( #1356 ) ) ;
#6989 = DIRECTION ( 'NONE',  ( -0.000000000000000000, -0.5735764363510414965, -0.8191520442889950182 ) ) ;
#6990 = FACE_OUTER_BOUND ( 'NONE', #13889, .T. ) ;
#6991 = CARTESIAN_POINT ( 'NONE',  ( 1.071796769724487675, -29.76257372698396964, -11.25009309380213551 ) ) ;
#6992 = EDGE_CURVE ( 'NONE', #2844, #6836, #7219, .T. ) ;
#6993 = CARTESIAN_POINT ( 'NONE',  ( 4.000000000000000000, 0.000000000000000000, 0.000000000000000000 ) ) ;
#6994 = CARTESIAN_POINT ( 'NONE',  ( 4.243569643750003451, -24.03347965934736763, -14.31337611479460037 ) ) ;
#6995 = VERTEX_POINT ( 'NONE', #5831 ) ;
#6996 = CARTESIAN_POINT ( 'NONE',  ( -1.734723475976807094E-15, 20.99999999999999289, -12.50000000000000000 ) ) ;
#6997 = CARTESIAN_POINT ( 'NONE',  ( -1.999999999999996225, -19.44407952440671039, -9.527020208913473454 ) ) ;
#6998 = CARTESIAN_POINT ( 'NONE',  ( -1.497042530366477164, 17.62180007765648071, 2.161531897785062384 ) ) ;
#6999 = ORIENTED_EDGE ( 'NONE', *, *, #14791, .T. ) ;
#7000 = FACE_OUTER_BOUND ( 'NONE', #12210, .T. ) ;
#7001 = CARTESIAN_POINT ( 'NONE',  ( -4.499999999999999112, 17.99680007765647005, 0.05647727720537927543 ) ) ;
#7002 = CARTESIAN_POINT ( 'NONE',  ( -9.000000000000003553, 34.19999999999999574, -2.500000000000001776 ) ) ;
#7003 = TOROIDAL_SURFACE ( 'NONE', #2868, 9.000000000000003553, 0.9999999999999991118 ) ;
#7004 = CARTESIAN_POINT ( 'NONE',  ( 0.8262555684460829442, 35.25319992234354771, -2.360188852285421302 ) ) ;
#7005 = VERTEX_POINT ( 'NONE', #12968 ) ;
#7006 = CARTESIAN_POINT ( 'NONE',  ( -5.330712181944246111E-15, -29.91450200949087801, -9.897876126833780930 ) ) ;
#7007 = CARTESIAN_POINT ( 'NONE',  ( 1.444289557196047680, 37.24680007765646650, 4.262301884875704161 ) ) ;
#7008 = ORIENTED_EDGE ( 'NONE', *, *, #17388, .F. ) ;
#7009 = CARTESIAN_POINT ( 'NONE',  ( 1.533898589781675205E-14, -27.25753381391755426, -7.672525335146852754 ) ) ;
#7010 = CARTESIAN_POINT ( 'NONE',  ( 1.071796769724504328, -24.60038579982458984, -3.877724695201188787 ) ) ;
#7011 = AXIS2_PLACEMENT_3D ( 'NONE', #1165, #8104, #10799 ) ;
#7012 = CARTESIAN_POINT ( 'NONE',  ( 8.673617379884035472E-15, 10.00000000000000000, 3.469446951953614189E-15 ) ) ;
#7013 = AXIS2_PLACEMENT_3D ( 'NONE', #4038, #9688, #13962 ) ;
#7014 = CARTESIAN_POINT ( 'NONE',  ( -2.121784821875005722, -26.35144522785700616, -6.945048742055040414 ) ) ;
#7015 = ORIENTED_EDGE ( 'NONE', *, *, #4382, .F. ) ;
#7016 = LINE ( 'NONE', #9808, #16262 ) ;
#7017 = ORIENTED_EDGE ( 'NONE', *, *, #16695, .T. ) ;
#7018 = CARTESIAN_POINT ( 'NONE',  ( -2.000000000000005773, -27.09817006914760640, -8.379240642573305919 ) ) ;
#7019 =( BOUNDED_CURVE ( )  B_SPLINE_CURVE ( 3, ( #9339, #9429, #15379, #10823 ),
 .UNSPECIFIED., .F., .T. ) 
 B_SPLINE_CURVE_WITH_KNOTS ( ( 4, 4 ),
 ( 4.712388980384689674, 6.283185307179586232 ),
 .UNSPECIFIED. ) 
 CURVE ( )  GEOMETRIC_REPRESENTATION_ITEM ( )  RATIONAL_B_SPLINE_CURVE ( ( 1.000000000000000000, 0.8047378541243649375, 0.8047378541243649375, 1.000000000000000000 ) ) 
 REPRESENTATION_ITEM ( '' )  );
#7020 = DIRECTION ( 'NONE',  ( 0.000000000000000000, -1.000000000000000000, 0.000000000000000000 ) ) ;
#7021 = CARTESIAN_POINT ( 'NONE',  ( 0.000000000000000000, 16.59999999999999787, 2.500000000000000000 ) ) ;
#7022 =( LENGTH_UNIT ( ) NAMED_UNIT ( * ) SI_UNIT ( .MILLI., .METRE. ) );
#7023 = CARTESIAN_POINT ( 'NONE',  ( -4.518350579753602325, 21.87819992234354416, 1.405661355842794391 ) ) ;
#7024 = AXIS2_PLACEMENT_3D ( 'NONE', #18060, #13668, #3849 ) ;
#7025 = CARTESIAN_POINT ( 'NONE',  ( 1.135272562821020070, 17.75319992234354771, -3.311245368580577164 ) ) ;
#7026 = CARTESIAN_POINT ( 'NONE',  ( -1.999999999999996225, -23.57382986613421139, -15.42491492779423723 ) ) ;
#7027 = CARTESIAN_POINT ( 'NONE',  ( -0.7188294034286043521, 37.49680007765647360, 2.395093729190366005 ) ) ;
#7028 = EDGE_CURVE ( 'NONE', #9017, #18266, #2627, .T. ) ;
#7029 = PRESENTATION_LAYER_ASSIGNMENT (  '', '', ( #15052 ) ) ;
#7030 = CARTESIAN_POINT ( 'NONE',  ( -2.733110507866328476, 32.37819992234353350, -3.862833514489096398 ) ) ;
#7031 = EDGE_CURVE ( 'NONE', #4433, #12491, #13574, .T. ) ;
#7032 = AXIS2_PLACEMENT_3D ( 'NONE', #5045, #3842, #2106 ) ;
#7033 = CARTESIAN_POINT ( 'NONE',  ( -2.000000000000005773, -26.25931453027926210, -7.181230776793885440 ) ) ;
#7034 = ORIENTED_EDGE ( 'NONE', *, *, #11920, .F. ) ;
#7035 = CARTESIAN_POINT ( 'NONE',  ( -1.055605843668875110, 15.00000000000000888, -3.337496964141338562 ) ) ;
#7036 = CARTESIAN_POINT ( 'NONE',  ( -2.864755990943265829, 23.24680007765647716, -2.011557305968488141 ) ) ;
#7037 = EDGE_CURVE ( 'NONE', #4895, #6401, #7060, .T. ) ;
#7038 = CARTESIAN_POINT ( 'NONE',  ( 4.243569643749997233, -25.25118226980542957, -7.509455447442163312 ) ) ;
#7039 = CARTESIAN_POINT ( 'NONE',  ( 0.05938372350929014415, 19.87180007765647716, 4.731580009072201776 ) ) ;
#7040 = CARTESIAN_POINT ( 'NONE',  ( -2.000000000000005773, -22.71031033106213570, -2.112727503762495296 ) ) ;
#7041 = AXIS2_PLACEMENT_3D ( 'NONE', #13834, #6871, #16731 ) ;
#7042 = CARTESIAN_POINT ( 'NONE',  ( 2.000000000000004441, -19.42257040733860762, -9.496302006245869620 ) ) ;
#7043 = ORIENTED_EDGE ( 'NONE', *, *, #137, .T. ) ;
#7044 = CIRCLE ( 'NONE', #5860, 8.000000000000001776 ) ;
#7045 = VERTEX_POINT ( 'NONE', #8514 ) ;
#7046 = CARTESIAN_POINT ( 'NONE',  ( -0.05938372350927861171, 23.62180007765647005, -3.680117784833935701 ) ) ;
#7047 = DIRECTION ( 'NONE',  ( 1.000000000000000000, 0.000000000000000000, 0.000000000000000000 ) ) ;
#7048 = DIRECTION ( 'NONE',  ( 0.000000000000000000, 0.000000000000000000, -1.000000000000000000 ) ) ;
#7049 = CARTESIAN_POINT ( 'NONE',  ( -1.071796769724496334, -24.68796655105670013, -4.002802970502292723 ) ) ;
#7050 = SURFACE_STYLE_USAGE ( .BOTH. , #12533 ) ;
#7051 = ORIENTED_EDGE ( 'NONE', *, *, #18132, .T. ) ;
#7052 = CARTESIAN_POINT ( 'NONE',  ( 3.500000000000000444, 23.25319992234354416, 0.05647727720529520379 ) ) ;
#7053 = CARTESIAN_POINT ( 'NONE',  ( 2.121784821874994176, -25.50183513151203130, -5.731679776451962915 ) ) ;
#7054 = CARTESIAN_POINT ( 'NONE',  ( -3.518350579753630747, 38.12180007765648071, -1.080741659609802729 ) ) ;
#7055 = CARTESIAN_POINT ( 'NONE',  ( -0.05938372350920063936, 23.87819992234354416, 3.680117784833935701 ) ) ;
#7056 = ADVANCED_FACE ( 'NONE', ( #1492 ), #7127, .F. ) ;
#7057 = CARTESIAN_POINT ( 'NONE',  ( -31.74999999999995737, 0.000000000000000000, 6.500000000000000000 ) ) ;
#7058 = AXIS2_PLACEMENT_3D ( 'NONE', #6276, #728, #16208 ) ;
#7059 = CARTESIAN_POINT ( 'NONE',  ( 4.243569643750000786, -22.73877416643638227, -8.192854934134281564 ) ) ;
#7060 = CIRCLE ( 'NONE', #9726, 2.149999999999999023 ) ;
#7061 = CARTESIAN_POINT ( 'NONE',  ( 0.000000000000000000, 3.000000000000000000, 0.000000000000000000 ) ) ;
#7062 = DIRECTION ( 'NONE',  ( -1.000000000000000000, -0.000000000000000000, -0.000000000000000000 ) ) ;
#7063 = CIRCLE ( 'NONE', #17155, 2.149999999999995470 ) ;
#7064 = CARTESIAN_POINT ( 'NONE',  ( -1.734723475976807094E-15, 29.79999999999999716, -2.500000000000000000 ) ) ;
#7065 = CARTESIAN_POINT ( 'NONE',  ( -2.121784821874996396, -17.54518305232318554, -7.182873304141986992 ) ) ;
#7066 = CYLINDRICAL_SURFACE ( 'NONE', #16281, 0.9999999999999991118 ) ;
#7067 = DIRECTION ( 'NONE',  ( 0.000000000000000000, -0.5735764363510414965, -0.8191520442889950182 ) ) ;
#7068 = ORIENTED_EDGE ( 'NONE', *, *, #18139, .T. ) ;
#7069 = AXIS2_PLACEMENT_3D ( 'NONE', #12467, #4134, #9604 ) ;
#7070 = CARTESIAN_POINT ( 'NONE',  ( -2.481649420246391902, 17.12819992234354416, -0.8687765177875723666 ) ) ;
#7071 = CARTESIAN_POINT ( 'NONE',  ( -4.243569643749997233, -24.72177138296861898, -15.29635856794139848 ) ) ;
#7072 = CARTESIAN_POINT ( 'NONE',  ( 3.500000000000000444, 36.74680007765648071, -0.05647727720536935281 ) ) ;
#7073 = CONTEXT_DEPENDENT_SHAPE_REPRESENTATION ( #11373, #9273 ) ;
#7074 = CARTESIAN_POINT ( 'NONE',  ( 8.399999999999998579, 0.000000000000000000, 0.000000000000000000 ) ) ;
#7075 = CARTESIAN_POINT ( 'NONE',  ( 8.500000000000019540, 10.00000000000000000, -22.49999999999999289 ) ) ;
#7076 = VERTEX_POINT ( 'NONE', #9078 ) ;
#7077 = CARTESIAN_POINT ( 'NONE',  ( -5.330712181944246111E-15, -24.49420468597354272, -2.156889308302777586 ) ) ;
#7078 = CARTESIAN_POINT ( 'NONE',  ( 1.027846397803542144, 31.24680007765647716, -3.346150245485522312 ) ) ;
#7079 = VECTOR ( 'NONE', #1613, 999.9999999999998863 ) ;
#7080 = CIRCLE ( 'NONE', #11516, 0.9999999999999991118 ) ;
#7081 = DIRECTION ( 'NONE',  ( -0.000000000000000000, -1.000000000000000000, -0.000000000000000000 ) ) ;
#7082 = CIRCLE ( 'NONE', #16599, 10.00000000000000178 ) ;
#7083 = CARTESIAN_POINT ( 'NONE',  ( -2.121784821875005722, -28.90027551689194496, -10.58515563886426136 ) ) ;
#7084 = DIRECTION ( 'NONE',  ( -1.000000000000000000, 0.000000000000000000, 4.336808689942021680E-16 ) ) ;
#7085 = CARTESIAN_POINT ( 'NONE',  ( -1.071796769724496334, -25.65587678669413663, -5.385122044233206395 ) ) ;
#7086 = DIRECTION ( 'NONE',  ( 0.000000000000000000, 0.000000000000000000, 1.000000000000000000 ) ) ;
#7087 = CARTESIAN_POINT ( 'NONE',  ( -2.121784821875005722, -28.38405672417600911, -9.847918799004165891 ) ) ;
#7088 = EDGE_LOOP ( 'NONE', ( #4527, #363, #12393, #10832 ) ) ;
#7089 = DIRECTION ( 'NONE',  ( -0.000000000000000000, 1.000000000000000000, -0.000000000000000000 ) ) ;
#7090 = CARTESIAN_POINT ( 'NONE',  ( 4.713407268011036227E-15, -15.93861937063522483, -6.533863231130032645 ) ) ;
#7091 = CARTESIAN_POINT ( 'NONE',  ( -1.497042530366477164, 22.62180007765647716, 2.161531897785062384 ) ) ;
#7092 = ORIENTED_EDGE ( 'NONE', *, *, #4316, .T. ) ;
#7093 = DIRECTION ( 'NONE',  ( 0.000000000000000000, 0.000000000000000000, 1.000000000000000000 ) ) ;
#7094 = EDGE_CURVE ( 'NONE', #13964, #9690, #575, .T. ) ;
#7095 = SURFACE_SIDE_STYLE ('',( #1194 ) ) ;
#7096 = AXIS2_PLACEMENT_3D ( 'NONE', #6889, #18148, #13661 ) ;
#7097 = DIRECTION ( 'NONE',  ( 0.000000000000000000, 0.000000000000000000, 1.000000000000000000 ) ) ;
#7098 = CARTESIAN_POINT ( 'NONE',  ( -2.500000000000001332, 34.50319992234354771, -0.05647727720530596601 ) ) ;
#7099 = EDGE_CURVE ( 'NONE', #9022, #11296, #7864, .T. ) ;
#7100 = ORIENTED_EDGE ( 'NONE', *, *, #2083, .T. ) ;
#7101 = CARTESIAN_POINT ( 'NONE',  ( -4.243569643750000786, -23.90026645004723704, -9.851637823819498152 ) ) ;
#7102 = CARTESIAN_POINT ( 'NONE',  ( -4.499999999999999112, 30.49680007765648071, 0.05647727720537927543 ) ) ;
#7103 = EDGE_CURVE ( 'NONE', #17729, #17010, #1168, .T. ) ;
#7104 = ORIENTED_EDGE ( 'NONE', *, *, #17293, .F. ) ;
#7105 = SURFACE_SIDE_STYLE ('',( #8410 ) ) ;
#7106 = EDGE_CURVE ( 'NONE', #11668, #4985, #14481, .T. ) ;
#7107 = DIRECTION ( 'NONE',  ( -4.915049848600951133E-16, 0.000000000000000000, -1.000000000000000000 ) ) ;
#7108 = CARTESIAN_POINT ( 'NONE',  ( 2.000000000000004441, -19.16446101098063792, -9.127683586315821884 ) ) ;
#7109 = VECTOR ( 'NONE', #17020, 1000.000000000000000 ) ;
#7110 = PLANE ( 'NONE',  #17783 ) ;
#7111 = CARTESIAN_POINT ( 'NONE',  ( 4.000000000000000888, -26.17485550509936942, -13.10008764894965871 ) ) ;
#7112 = CARTESIAN_POINT ( 'NONE',  ( -4.243569643750005227, -23.56271663529704696, -5.098076617066438665 ) ) ;
#7113 = ORIENTED_EDGE ( 'NONE', *, *, #141, .F. ) ;
#7114 = CARTESIAN_POINT ( 'NONE',  ( -8.500000000000007105, 14.80000000000000071, -22.69999999999999929 ) ) ;
#7115 = EDGE_LOOP ( 'NONE', ( #4626, #3155, #16825, #10215 ) ) ;
#7116 = ORIENTED_EDGE ( 'NONE', *, *, #8542, .T. ) ;
#7117 = FACE_OUTER_BOUND ( 'NONE', #12464, .T. ) ;
#7118 = CARTESIAN_POINT ( 'NONE',  ( -3.673772985318163098, 16.75319992234354416, 2.599342558261029001 ) ) ;
#7119 = CARTESIAN_POINT ( 'NONE',  ( -2.798362969681409851, 29.75319992234354416, -2.102939460078765421 ) ) ;
#7120 = CARTESIAN_POINT ( 'NONE',  ( -3.999999999999997335, -24.75630545268398208, -15.10050612620725197 ) ) ;
#7121 = CARTESIAN_POINT ( 'NONE',  ( 0.8262555684461332373, 39.74680007765648071, 2.360188852285403982 ) ) ;
#7122 = VECTOR ( 'NONE', #17129, 1000.000000000000000 ) ;
#7123 = CARTESIAN_POINT ( 'NONE',  ( 4.518350579753602325, 35.62819992234354771, -1.405661355842793725 ) ) ;
#7124 = CARTESIAN_POINT ( 'NONE',  ( -4.000000000000004441, -25.07683894372948785, -7.505639578380876031 ) ) ;
#7125 = EDGE_LOOP ( 'NONE', ( #17051, #10261, #7653, #9888, #6693 ) ) ;
#7126 = AXIS2_PLACEMENT_3D ( 'NONE', #9866, #10041, #8467 ) ;
#7127 = CYLINDRICAL_SURFACE ( 'NONE', #3814, 4.000000000000000000 ) ;
#7128 = CARTESIAN_POINT ( 'NONE',  ( -2.115076519116362519, 22.62180007765647360, 3.012182706137107147 ) ) ;
#7129 = CARTESIAN_POINT ( 'NONE',  ( 9.609723682702158598, -9.971172948454899654, 12.03203570040726511 ) ) ;
#7130 = CARTESIAN_POINT ( 'NONE',  ( -2.121784821874996396, -19.61005822318693248, -10.13182066358236888 ) ) ;
#7131 = CARTESIAN_POINT ( 'NONE',  ( -1.444289557196047014, 25.99680007765648071, -4.262301884875704161 ) ) ;
#7132 = AXIS2_PLACEMENT_3D ( 'NONE', #16380, #14811, #797 ) ;
#7133 = CARTESIAN_POINT ( 'NONE',  ( 3.061616997868382648E-16, 5.000000000000000000, 2.499999999999999556 ) ) ;
#7134 = VERTEX_POINT ( 'NONE', #13522 ) ;
#7135 = ORIENTED_EDGE ( 'NONE', *, *, #15672, .F. ) ;
#7136 = CARTESIAN_POINT ( 'NONE',  ( -3.481649420246369697, 20.37180007765647716, 1.193696214020542490 ) ) ;
#7137 = EDGE_CURVE ( 'NONE', #16218, #10036, #12106, .T. ) ;
#7138 = CARTESIAN_POINT ( 'NONE',  ( -7.191589934391292793, -10.00000000000000178, 14.52136967842657000 ) ) ;
#7139 = DIRECTION ( 'NONE',  ( 0.000000000000000000, 0.000000000000000000, -1.000000000000000000 ) ) ;
#7140 = CARTESIAN_POINT ( 'NONE',  ( -1.071796769724486564, -27.72075195755788712, -8.334069403673582954 ) ) ;
#7141 = PRESENTATION_STYLE_ASSIGNMENT (( #7050 ) ) ;
#7142 = ORIENTED_EDGE ( 'NONE', *, *, #5297, .F. ) ;
#7143 = CARTESIAN_POINT ( 'NONE',  ( 0.05938372350920109732, 20.12819992234353705, -3.680117784833935701 ) ) ;
#7144 = CARTESIAN_POINT ( 'NONE',  ( -2.121784821874996396, -19.35194882682896633, -9.763202243652322920 ) ) ;
#7145 = CARTESIAN_POINT ( 'NONE',  ( 2.481649420246374138, 16.62180007765648071, -0.8687765177876252132 ) ) ;
#7146 = CARTESIAN_POINT ( 'NONE',  ( -1.027846397803611866, 35.00319992234354771, -3.346150245485499219 ) ) ;
#7147 = FACE_OUTER_BOUND ( 'NONE', #16231, .T. ) ;
#7148 = CARTESIAN_POINT ( 'NONE',  ( 2.000000000000004441, -22.06819172071273272, -13.27464081153562425 ) ) ;
#7149 = CARTESIAN_POINT ( 'NONE',  ( -5.330712181944245322E-15, -27.33340804591119522, -6.211691927533303570 ) ) ;
#7150 = CIRCLE ( 'NONE', #14895, 4.000000000000000000 ) ;
#7151 = CARTESIAN_POINT ( 'NONE',  ( -3.122678035296125643, -15.23680830283799281, -9.380745725236772969 ) ) ;
#7152 = EDGE_CURVE ( 'NONE', #17369, #634, #2372, .T. ) ;
#7153 = AXIS2_PLACEMENT_3D ( 'NONE', #10286, #4277, #17277 ) ;
#7154 = DIRECTION ( 'NONE',  ( -0.000000000000000000, -0.5735764363510414965, -0.8191520442889950182 ) ) ;
#7155 = AXIS2_PLACEMENT_3D ( 'NONE', #10481, #579, #1786 ) ;
#7156 = EDGE_CURVE ( 'NONE', #5293, #17312, #7686, .T. ) ;
#7157 = CARTESIAN_POINT ( 'NONE',  ( -8.000000000000001776, 43.00000000000000000, 2.499999999999998224 ) ) ;
#7158 = CARTESIAN_POINT ( 'NONE',  ( 4.243569643750000786, -20.64163532102788778, -5.197830272202643265 ) ) ;
#7159 = CARTESIAN_POINT ( 'NONE',  ( -8.999999999999996447, -10.00000000000000000, 30.00000000000000000 ) ) ;
#7160 = AXIS2_PLACEMENT_3D ( 'NONE', #2207, #16199, #7924 ) ;
#7161 = EDGE_CURVE ( 'NONE', #11263, #1346, #10032, .T. ) ;
#7162 = ORIENTED_EDGE ( 'NONE', *, *, #14586, .T. ) ;
#7163 = CARTESIAN_POINT ( 'NONE',  ( -2.055738996568281518, 24.25319992234354061, 1.423772053676066962 ) ) ;
#7164 = CARTESIAN_POINT ( 'NONE',  ( 4.243569643750000786, -27.09437022997710187, -14.41329077045383578 ) ) ;
#7165 = DIRECTION ( 'NONE',  ( 0.000000000000000000, 0.000000000000000000, 1.000000000000000000 ) ) ;
#7166 = CARTESIAN_POINT ( 'NONE',  ( -9.356479678992938531, -9.999999999999996447, 13.59332006026303574 ) ) ;
#7167 = FACE_OUTER_BOUND ( 'NONE', #8417, .T. ) ;
#7168 = ORIENTED_EDGE ( 'NONE', *, *, #10045, .F. ) ;
#7169 = AXIS2_PLACEMENT_3D ( 'NONE', #15945, #84, #5737 ) ;
#7170 = CARTESIAN_POINT ( 'NONE',  ( -4.243569643750004339, -22.27216965350720557, -3.254984517416200873 ) ) ;
#7171 = CARTESIAN_POINT ( 'NONE',  ( -1.027846397803541700, 29.99680007765648071, 3.346150245485522312 ) ) ;
#7172 = VECTOR ( 'NONE', #7388, 1000.000000000000000 ) ;
#7173 = CARTESIAN_POINT ( 'NONE',  ( -1.999999999999996225, -17.05656760739055500, -6.117299823553768334 ) ) ;
#7174 = FILL_AREA_STYLE_COLOUR ( '', #15185 ) ;
#7175 = CARTESIAN_POINT ( 'NONE',  ( 2.121784821874994176, -28.08292909509171764, -9.417863975752439387 ) ) ;
#7176 = DIRECTION ( 'NONE',  ( -0.000000000000000000, -1.000000000000000000, -0.000000000000000000 ) ) ;
#7177 = CARTESIAN_POINT ( 'NONE',  ( -4.000000000000004441, -26.43191327531376800, -9.440886284020393759 ) ) ;
#7178 = CARTESIAN_POINT ( 'NONE',  ( 8.000000000000000000, 25.39999999999999503, -2.500000000000000888 ) ) ;
#7179 = CARTESIAN_POINT ( 'NONE',  ( -5.330712181944245322E-15, -28.07547256044035322, -7.271469884832189479 ) ) ;
#7180 = VECTOR ( 'NONE', #16055, 1000.000000000000000 ) ;
#7181 = CARTESIAN_POINT ( 'NONE',  ( 2.694913683823408235, -15.45745613286698550, -10.86990606519495195 ) ) ;
#7182 = CIRCLE ( 'NONE', #1578, 8.000000000000003553 ) ;
#7183 = CARTESIAN_POINT ( 'NONE',  ( -2.000000000000005773, -23.48463852013604480, -3.218582763552638948 ) ) ;
#7184 =( GEOMETRIC_REPRESENTATION_CONTEXT ( 3 ) GLOBAL_UNCERTAINTY_ASSIGNED_CONTEXT ( ( #18263 ) ) GLOBAL_UNIT_ASSIGNED_CONTEXT ( ( #2338, #4069, #7874 ) ) REPRESENTATION_CONTEXT ( 'NONE', 'WORKASPACE' ) );
#7185 = CARTESIAN_POINT ( 'NONE',  ( -2.518350579753628526, 20.62180007765647716, -0.7558219633769075463 ) ) ;
#7186 = ORIENTED_EDGE ( 'NONE', *, *, #1434, .F. ) ;
#7187 = CARTESIAN_POINT ( 'NONE',  ( 3.518350579753631191, 21.87180007765647360, 1.080741659609802729 ) ) ;
#7188 = CARTESIAN_POINT ( 'NONE',  ( 9.000000000000000000, 25.39999999999999503, -2.500000000000001332 ) ) ;
#7189 = EDGE_CURVE ( 'NONE', #9963, #9627, #17779, .T. ) ;
#7190 = DIRECTION ( 'NONE',  ( 0.000000000000000000, 0.000000000000000000, -1.000000000000000000 ) ) ;
#7191 = CARTESIAN_POINT ( 'NONE',  ( -2.055738996568281518, 36.75319992234354771, 1.423772053676066962 ) ) ;
#7192 = ORIENTED_EDGE ( 'NONE', *, *, #15238, .F. ) ;
#7193 = CARTESIAN_POINT ( 'NONE',  ( -4.243569643749998122, -21.65672230121773723, -10.91901483127208294 ) ) ;
#7194 = CARTESIAN_POINT ( 'NONE',  ( 1.336863392178479160, 33.74680007765647360, -4.297206761780677731 ) ) ;
#7195 = VERTEX_POINT ( 'NONE', #14665 ) ;
#7196 = AXIS2_PLACEMENT_3D ( 'NONE', #12462, #6718, #13581 ) ;
#7197 = CARTESIAN_POINT ( 'NONE',  ( -6.938893903907228378E-15, 6.938893903907228378E-15, 30.00000000000000000 ) ) ;
#7198 = CARTESIAN_POINT ( 'NONE',  ( -1.071796769724477238, -25.72040413648858603, -5.477276650222477450 ) ) ;
#7199 = DIRECTION ( 'NONE',  ( 0.000000000000000000, 0.5000000000000002220, 0.8660254037844384856 ) ) ;
#7200 = CARTESIAN_POINT ( 'NONE',  ( -2.000000000000005773, -28.64682644729541749, -10.59095116215359234 ) ) ;
#7201 = CARTESIAN_POINT ( 'NONE',  ( 1.071796769724485232, -29.50446433062600349, -10.88147467387208955 ) ) ;
#7202 = CARTESIAN_POINT ( 'NONE',  ( -5.330712181944245322E-15, -26.04286106412135027, -4.368599827883064890 ) ) ;
#7203 = EDGE_CURVE ( 'NONE', #5462, #17357, #2948, .T. ) ;
#7204 = ORIENTED_EDGE ( 'NONE', *, *, #10999, .T. ) ;
#7205 = DIRECTION ( 'NONE',  ( -1.000000000000000000, 0.000000000000000000, 4.336808689942021680E-16 ) ) ;
#7206 = ORIENTED_EDGE ( 'NONE', *, *, #7600, .T. ) ;
#7207 = EDGE_LOOP ( 'NONE', ( #3004, #5811, #9918, #15639 ) ) ;
#7208 = CYLINDRICAL_SURFACE ( 'NONE', #74, 4.000000000000000000 ) ;
#7209 = EDGE_CURVE ( 'NONE', #12253, #15689, #17179, .T. ) ;
#7210 = CIRCLE ( 'NONE', #6908, 8.000000000000001776 ) ;
#7211 = CARTESIAN_POINT ( 'NONE',  ( 0.000000000000000000, 0.000000000000000000, 3.799999999999999378 ) ) ;
#7212 = CARTESIAN_POINT ( 'NONE',  ( 2.733110507866328920, 16.12819992234354416, 3.862833514489095510 ) ) ;
#7213 = CARTESIAN_POINT ( 'NONE',  ( -3.500000000000000444, 27.00319992234354771, -0.05647727720529563400 ) ) ;
#7214 = CARTESIAN_POINT ( 'NONE',  ( 1.497042530366477164, 38.87180007765646650, -2.161531897785062384 ) ) ;
#7215 = ORIENTED_EDGE ( 'NONE', *, *, #6010, .T. ) ;
#7216 = CARTESIAN_POINT ( 'NONE',  ( 4.499999999999999112, 30.75319992234354416, 0.05647727720528474687 ) ) ;
#7217 = CARTESIAN_POINT ( 'NONE',  ( 1.999999999999994449, -26.21629629755294033, -7.119794373472207560 ) ) ;
#7218 = ORIENTED_EDGE ( 'NONE', *, *, #13174, .T. ) ;
#7219 = LINE ( 'NONE', #11298, #4684 ) ;
#7220 = CARTESIAN_POINT ( 'NONE',  ( -3.500000000000000444, 27.99680007765648071, 0.05647727720536892260 ) ) ;
#7221 = CARTESIAN_POINT ( 'NONE',  ( -4.551717183842042047, -10.00000000000000000, -2.180355508048917201 ) ) ;
#7222 = CARTESIAN_POINT ( 'NONE',  ( -4.243569643749998122, -20.59202104124112154, -9.398463849060636477 ) ) ;
#7223 = CARTESIAN_POINT ( 'NONE',  ( 1.336863392178479160, 31.24680007765648071, -4.297206761780677731 ) ) ;
#7224 = ADVANCED_FACE ( 'NONE', ( #14568 ), #1768, .T. ) ;
#7225 = ORIENTED_EDGE ( 'NONE', *, *, #17505, .T. ) ;
#7226 = EDGE_LOOP ( 'NONE', ( #10360, #14482, #7585, #16309 ) ) ;
#7227 = CARTESIAN_POINT ( 'NONE',  ( 0.05938372350927906274, 27.37180007765647716, 3.680117784833935701 ) ) ;
#7228 = DIRECTION ( 'NONE',  ( -0.000000000000000000, -1.000000000000000000, -0.000000000000000000 ) ) ;
#7229 = CARTESIAN_POINT ( 'NONE',  ( -3.999999999999997335, -19.59411752552461294, -7.728137727606295471 ) ) ;
#7230 = FILL_AREA_STYLE ('',( #10385 ) ) ;
#7231 = ORIENTED_EDGE ( 'NONE', *, *, #10999, .F. ) ;
#7232 = CARTESIAN_POINT ( 'NONE',  ( 2.211161402132839626, 20.37819992234354416, -2.942372952327218183 ) ) ;
#7233 = DIRECTION ( 'NONE',  ( -0.000000000000000000, -1.000000000000000000, -0.000000000000000000 ) ) ;
#7234 = CARTESIAN_POINT ( 'NONE',  ( 4.243569643749996345, -24.73496347708949017, -6.772218607582066952 ) ) ;
#7235 = CARTESIAN_POINT ( 'NONE',  ( -0.05938372350927861171, 36.12180007765648782, -3.680117784833935701 ) ) ;
#7236 = APPLICATION_CONTEXT ( 'automotive_design' ) ;
#7237 = CARTESIAN_POINT ( 'NONE',  ( 2.798362969681409851, 31.00319992234354416, 2.102939460078764977 ) ) ;
#7238 = PLANE ( 'NONE',  #2264 ) ;
#7239 = DIRECTION ( 'NONE',  ( 0.000000000000000000, 0.000000000000000000, 1.000000000000000000 ) ) ;
#7240 = CARTESIAN_POINT ( 'NONE',  ( 4.243569643750003451, -20.71032118123852683, -9.567413958195238877 ) ) ;
#7241 = CARTESIAN_POINT ( 'NONE',  ( 0.000000000000000000, 4.000000000000007105, 4.000000000000000000 ) ) ;
#7242 = CARTESIAN_POINT ( 'NONE',  ( -3.108848142585320939, -10.00000000000000178, -11.78746955954697739 ) ) ;
#7243 = DIRECTION ( 'NONE',  ( 0.8191520442889951292, 0.4698463103929521600, -0.3289899283371603422 ) ) ;
#7244 = CARTESIAN_POINT ( 'NONE',  ( 8.000000000000000000, 20.99999999999999289, -2.500000000000000888 ) ) ;
#7245 = CARTESIAN_POINT ( 'NONE',  ( 2.121784821875004390, -17.07198249233357856, -6.507072867603563182 ) ) ;
#7246 = CARTESIAN_POINT ( 'NONE',  ( -1.055605843668875110, 15.00000000000000888, -3.337496964141338562 ) ) ;
#7247 = DIRECTION ( 'NONE',  ( 0.000000000000000000, 0.000000000000000000, 1.000000000000000000 ) ) ;
#7248 = ORIENTED_EDGE ( 'NONE', *, *, #11882, .T. ) ;
#7249 = CARTESIAN_POINT ( 'NONE',  ( -0.7188294034286550893, 20.00319992234354771, -2.395093729190349130 ) ) ;
#7250 = CARTESIAN_POINT ( 'NONE',  ( -2.121784821875005722, -29.67460370596585406, -11.69101089865440457 ) ) ;
#7251 = CARTESIAN_POINT ( 'NONE',  ( 3.518350579753631191, 16.87180007765648071, 1.080741659609802285 ) ) ;
#7252 = DIRECTION ( 'NONE',  ( -1.000000000000000000, -0.000000000000000000, -0.000000000000000000 ) ) ;
#7253 = DIRECTION ( 'NONE',  ( 8.673617379884034239E-17, 0.000000000000000000, 1.000000000000000000 ) ) ;
#7254 = EDGE_CURVE ( 'NONE', #8704, #17065, #13157, .T. ) ;
#7255 = ORIENTED_EDGE ( 'NONE', *, *, #3864, .F. ) ;
#7256 = CARTESIAN_POINT ( 'NONE',  ( 4.243569643750003451, -18.12922721765884049, -5.881229758894760629 ) ) ;
#7257 = CARTESIAN_POINT ( 'NONE',  ( 2.864755990943265829, 34.49680007765648071, 2.011557305968487697 ) ) ;
#7258 = CARTESIAN_POINT ( 'NONE',  ( 2.121784821874994176, -29.40573975142631014, -11.30703337789393359 ) ) ;
#7259 = EDGE_CURVE ( 'NONE', #9627, #4165, #467, .T. ) ;
#7260 = EDGE_CURVE ( 'NONE', #1058, #14161, #11761, .T. ) ;
#7261 = DIRECTION ( 'NONE',  ( -4.915049848600951133E-16, 0.000000000000000000, -1.000000000000000000 ) ) ;
#7262 = CARTESIAN_POINT ( 'NONE',  ( -4.243569643749998122, -23.68933379753673663, -13.82188488822120753 ) ) ;
#7263 = CIRCLE ( 'NONE', #9589, 3.799999999999999378 ) ;
#7264 = FACE_OUTER_BOUND ( 'NONE', #3165, .T. ) ;
#7265 = EDGE_CURVE ( 'NONE', #244, #12707, #750, .T. ) ;
#7266 = FACE_OUTER_BOUND ( 'NONE', #7305, .T. ) ;
#7267 = CARTESIAN_POINT ( 'NONE',  ( -9.000000000000001776, 27.59999999999999432, 2.499999999999998224 ) ) ;
#7268 = VECTOR ( 'NONE', #11425, 1000.000000000000000 ) ;
#7269 = CARTESIAN_POINT ( 'NONE',  ( 2.121784821874994176, -28.08292909509171764, -9.417863975752439387 ) ) ;
#7270 = DIRECTION ( 'NONE',  ( -0.000000000000000000, -0.5735764363510414965, -0.8191520442889950182 ) ) ;
#7271 = CARTESIAN_POINT ( 'NONE',  ( 4.713407268011036227E-15, -16.97105695606709830, -8.008336910850223589 ) ) ;
#7272 = CARTESIAN_POINT ( 'NONE',  ( -0.7188294034286043521, 22.49680007765648071, 2.395093729190366005 ) ) ;
#7273 = EDGE_LOOP ( 'NONE', ( #6082, #15993, #4567, #17659 ) ) ;
#7274 = CARTESIAN_POINT ( 'NONE',  ( -2.211161402132901799, 25.87180007765647360, -2.942372952327172886 ) ) ;
#7275 = EDGE_CURVE ( 'NONE', #3130, #1326, #2146, .T. ) ;
#7276 = CARTESIAN_POINT ( 'NONE',  ( -4.000000000000000888, -23.78734358949309424, -9.690367265603486047 ) ) ;
#7277 = CARTESIAN_POINT ( 'NONE',  ( 0.000000000000000000, 0.000000000000000000, 0.000000000000000000 ) ) ;
#7278 = DIRECTION ( 'NONE',  ( -0.000000000000000000, -1.000000000000000000, -0.000000000000000000 ) ) ;
#7279 = CARTESIAN_POINT ( 'NONE',  ( 2.500000000000001332, 33.25319992234354771, 0.05647727720530566764 ) ) ;
#7280 = VERTEX_POINT ( 'NONE', #6395 ) ;
#7281 = CARTESIAN_POINT ( 'NONE',  ( 2.121784821874994176, -27.08275518420459349, -7.989467598523504854 ) ) ;
#7282 = CARTESIAN_POINT ( 'NONE',  ( -4.518350579753632523, 30.62180007765647005, -1.405661355842698468 ) ) ;
#7283 = TOROIDAL_SURFACE ( 'NONE', #12628, 9.000000000000001776, 0.9999999999999991118 ) ;
#7284 = ORIENTED_EDGE ( 'NONE', *, *, #7094, .T. ) ;
#7285 = DIRECTION ( 'NONE',  ( 0.000000000000000000, 0.000000000000000000, 1.000000000000000000 ) ) ;
#7286 = CARTESIAN_POINT ( 'NONE',  ( 2.121784821875004390, -22.52454349039567205, -14.29413698862582294 ) ) ;
#7287 = DIRECTION ( 'NONE',  ( 0.000000000000000000, 0.000000000000000000, 1.000000000000000000 ) ) ;
#7288 = FACE_OUTER_BOUND ( 'NONE', #14278, .T. ) ;
#7289 = LINE ( 'NONE', #5730, #8206 ) ;
#7290 =( BOUNDED_CURVE ( )  B_SPLINE_CURVE ( 2, ( #15465, #2759, #3116, #1821, #8749, #12924, #10517, #6065, #10329 ),
 .UNSPECIFIED., .F., .T. ) 
 B_SPLINE_CURVE_WITH_KNOTS ( ( 3, 2, 2, 2, 3 ),
 ( 0.1293103448275862155, 0.1321839080459770166, 0.1379310344827586188, 0.1436781609195402210, 0.1465517241379310498 ),
 .UNSPECIFIED. ) 
 CURVE ( )  GEOMETRIC_REPRESENTATION_ITEM ( )  RATIONAL_B_SPLINE_CURVE ( ( 0.9330127018922194093, 0.9330127018922194093, 1.000000000000000000, 0.8660254037844387076, 1.000000000000000000, 0.8660254037844387076, 1.000000000000000000, 0.9330127018922189652, 0.9330127018922192983 ) ) 
 REPRESENTATION_ITEM ( '' )  );
#7291 = CARTESIAN_POINT ( 'NONE',  ( -5.330712181944245322E-15, -25.52664227140541797, -3.631362988022969862 ) ) ;
#7292 = ORIENTED_EDGE ( 'NONE', *, *, #150, .F. ) ;
#7293 = CYLINDRICAL_SURFACE ( 'NONE', #14449, 6.499999999999999112 ) ;
#7294 = VERTEX_POINT ( 'NONE', #3612 ) ;
#7295 = CIRCLE ( 'NONE', #17706, 10.00000000000000178 ) ;
#7296 = ORIENTED_EDGE ( 'NONE', *, *, #1520, .T. ) ;
#7297 = DIRECTION ( 'NONE',  ( 0.000000000000000000, 0.000000000000000000, 1.000000000000000000 ) ) ;
#7298 = CARTESIAN_POINT ( 'NONE',  ( -9.000000000000001776, 23.19999999999999574, 2.499999999999998224 ) ) ;
#7299 = CARTESIAN_POINT ( 'NONE',  ( 0.05938372350919016857, 20.12819992234354416, -4.731580009072201776 ) ) ;
#7300 = CARTESIAN_POINT ( 'NONE',  ( 3.481649420246395010, 25.87819992234354771, 1.193696214020467439 ) ) ;
#7301 = CARTESIAN_POINT ( 'NONE',  ( -2.500000000000001332, 37.99680007765646650, 0.05647727720535858364 ) ) ;
#7302 = ORIENTED_EDGE ( 'NONE', *, *, #11437, .T. ) ;
#7303 = CARTESIAN_POINT ( 'NONE',  ( 2.829195390882724759, 30.37819992234354061, -3.793023760679264278 ) ) ;
#7304 = CARTESIAN_POINT ( 'NONE',  ( -2.000000000000005773, -26.00120513392129240, -6.812612356863837704 ) ) ;
#7305 = EDGE_LOOP ( 'NONE', ( #11922, #8056, #6759, #3763 ) ) ;
#7306 = AXIS2_PLACEMENT_3D ( 'NONE', #5005, #3444, #16153 ) ;
#7307 = CARTESIAN_POINT ( 'NONE',  ( -9.000000000000001776, 34.19999999999999574, 2.499999999999998224 ) ) ;
#7308 = CIRCLE ( 'NONE', #12349, 8.000000000000001776 ) ;
#7309 = CARTESIAN_POINT ( 'NONE',  ( -3.500000000000000444, 30.49680007765647716, 0.05647727720536892260 ) ) ;
#7310 = CARTESIAN_POINT ( 'NONE',  ( 1.533898589781675205E-14, -27.19300646412311551, -7.580370729157575482 ) ) ;
#7311 = CARTESIAN_POINT ( 'NONE',  ( -4.243569643750000786, -21.02879941556483345, -5.750757902097718421 ) ) ;
#7312 = CARTESIAN_POINT ( 'NONE',  ( -0.05938372350928957516, 31.12180007765647716, -4.731580009072201776 ) ) ;
#7313 = DIRECTION ( 'NONE',  ( -1.000000000000000000, 0.000000000000000000, 0.000000000000000000 ) ) ;
#7314 = ORIENTED_EDGE ( 'NONE', *, *, #13044, .T. ) ;
#7315 = VERTEX_POINT ( 'NONE', #12038 ) ;
#7316 = CARTESIAN_POINT ( 'NONE',  ( 2.798362969681366330, 23.99680007765647716, -2.102939460078824929 ) ) ;
#7317 = CARTESIAN_POINT ( 'NONE',  ( 12.00000000000000178, 13.00000000000000178, 15.00000000000000000 ) ) ;
#7318 = SURFACE_STYLE_FILL_AREA ( #17279 ) ;
#7319 = CARTESIAN_POINT ( 'NONE',  ( -4.000000000000004441, -26.36738592551933280, -9.348731678031116488 ) ) ;
#7320 = EDGE_LOOP ( 'NONE', ( #13330, #1041 ) ) ;
#7321 = AXIS2_PLACEMENT_3D ( 'NONE', #12551, #16752, #7247 ) ;
#7322 = CARTESIAN_POINT ( 'NONE',  ( -3.518350579753605434, 19.37819992234354416, 1.080741659609877781 ) ) ;
#7323 = CARTESIAN_POINT ( 'NONE',  ( 3.999999999999996447, -27.63642379165096585, -11.16110557702728023 ) ) ;
#7324 = CIRCLE ( 'NONE', #7032, 0.9999999999999991118 ) ;
#7325 = CARTESIAN_POINT ( 'NONE',  ( -4.243569643750000786, -22.83556519007061425, -8.331086841608051685 ) ) ;
#7326 =( BOUNDED_CURVE ( )  B_SPLINE_CURVE ( 2, ( #15353, #986, #14036, #13856, #1164, #15168, #9491, #18150, #2473 ),
 .UNSPECIFIED., .F., .F. ) 
 B_SPLINE_CURVE_WITH_KNOTS ( ( 3, 2, 2, 2, 3 ),
 ( 0.04310344827586207184, 0.04597701149425287293, 0.05172413793103448204, 0.05747126436781609116, 0.06034482758620690612 ),
 .UNSPECIFIED. ) 
 CURVE ( )  GEOMETRIC_REPRESENTATION_ITEM ( )  RATIONAL_B_SPLINE_CURVE ( ( 0.9330127018922194093, 0.9330127018922194093, 1.000000000000000000, 0.8660254037844387076, 1.000000000000000000, 0.8660254037844387076, 1.000000000000000000, 0.9330127018922191873, 0.9330127018922194093 ) ) 
 REPRESENTATION_ITEM ( '' )  );
#7327 = CARTESIAN_POINT ( 'NONE',  ( 0.8262555684461332373, 17.24680007765648071, 2.360188852285403982 ) ) ;
#7328 = ADVANCED_FACE ( 'NONE', ( #17732 ), #4998, .F. ) ;
#7329 = CARTESIAN_POINT ( 'NONE',  ( -3.481649420246394122, 34.62819992234354771, -1.193696214020467883 ) ) ;
#7330 = CARTESIAN_POINT ( 'NONE',  ( 4.000000000000000888, -19.78664794594458698, -3.976781756687743918 ) ) ;
#7331 = CARTESIAN_POINT ( 'NONE',  ( 1.071796769724485454, -21.61922704757731140, -13.56776313036627002 ) ) ;
#7332 = CARTESIAN_POINT ( 'NONE',  ( -5.330712181944245322E-15, -26.81718925319525937, -5.474455087673208986 ) ) ;
#7333 = AXIS2_PLACEMENT_3D ( 'NONE', #5779, #4481, #17112 ) ;
#7334 = ADVANCED_FACE ( 'NONE', ( #3972 ), #3833, .T. ) ;
#7335 = CARTESIAN_POINT ( 'NONE',  ( -6.808698206972851885, -11.94148469789129763, 12.85951478023477712 ) ) ;
#7336 = MECHANICAL_DESIGN_GEOMETRIC_PRESENTATION_REPRESENTATION (  '', ( #17434 ), #9707 ) ;
#7337 = EDGE_CURVE ( 'NONE', #2970, #9801, #14521, .T. ) ;
#7338 = CARTESIAN_POINT ( 'NONE',  ( -4.551717183842047376, -10.00000000000000178, -2.180355508048917201 ) ) ;
#7339 = DIRECTION ( 'NONE',  ( 0.000000000000000000, 0.000000000000000000, 1.000000000000000000 ) ) ;
#7340 = DIRECTION ( 'NONE',  ( -0.000000000000000000, -1.000000000000000000, -0.000000000000000000 ) ) ;
#7341 = CARTESIAN_POINT ( 'NONE',  ( 4.243569643749996345, -22.15386951350980738, -3.086034408281590036 ) ) ;
#7342 = CARTESIAN_POINT ( 'NONE',  ( 0.000000000000000000, 9.254131787996968228, 30.52396275209373044 ) ) ;
#7343 = FACE_BOUND ( 'NONE', #16900, .T. ) ;
#7344 = ORIENTED_EDGE ( 'NONE', *, *, #12378, .F. ) ;
#7345 = CARTESIAN_POINT ( 'NONE',  ( -1.497042530366522461, 19.87819992234354771, -2.161531897785030409 ) ) ;
#7346 = CARTESIAN_POINT ( 'NONE',  ( -4.000000000000000888, -22.17415986155084795, -7.386502140033922359 ) ) ;
#7347 = CARTESIAN_POINT ( 'NONE',  ( 2.115076519116362963, 16.37180007765647716, -3.012182706137107147 ) ) ;
#7348 = CARTESIAN_POINT ( 'NONE',  ( 0.05938372350929014415, 17.37180007765647716, 4.731580009072201776 ) ) ;
#7349 = AXIS2_PLACEMENT_3D ( 'NONE', #2329, #7958, #3789 ) ;
#7350 = CARTESIAN_POINT ( 'NONE',  ( -9.933259399355584662, -9.929220090424015766, 8.891678395390737677 ) ) ;
#7351 = CONICAL_SURFACE ( 'NONE', #13539, 2.000000000000001776, 1.029744260000000189 ) ;
#7352 = CARTESIAN_POINT ( 'NONE',  ( 6.262826437386884493, -14.35615764868780708, -3.437201991564796444 ) ) ;
#7353 = ORIENTED_EDGE ( 'NONE', *, *, #9800, .F. ) ;
#7354 = CARTESIAN_POINT ( 'NONE',  ( -4.243569643750004339, -21.75595086079126261, -2.517747677556105845 ) ) ;
#7355 = CARTESIAN_POINT ( 'NONE',  ( 2.211161402132902243, 39.62180007765646650, 2.942372952327172442 ) ) ;
#7356 = CARTESIAN_POINT ( 'NONE',  ( -4.243569643749997233, -25.01214445387132912, -15.71105429036270351 ) ) ;
#7357 = CARTESIAN_POINT ( 'NONE',  ( 4.730628863548789710E-15, -21.46729876507041013, -14.91998009733462816 ) ) ;
#7358 = CARTESIAN_POINT ( 'NONE',  ( 2.610818894029696136, -22.30731640688717121, -2.152030296976241708 ) ) ;
#7359 = AXIS2_PLACEMENT_3D ( 'NONE', #10836, #7962, #7867 ) ;
#7360 = CARTESIAN_POINT ( 'NONE',  ( 4.000000000000000000, 0.000000000000000000, 0.000000000000000000 ) ) ;
#7361 = CARTESIAN_POINT ( 'NONE',  ( 1.300000000000000044, 1.443375672974065216, 7.222237291452134449E-31 ) ) ;
#7362 = CARTESIAN_POINT ( 'NONE',  ( -2.121784821875005722, -27.09350974238616416, -8.004826699353927211 ) ) ;
#7363 = ADVANCED_FACE ( 'NONE', ( #8047 ), #5177, .F. ) ;
#7364 = CARTESIAN_POINT ( 'NONE',  ( 3.999999999999996447, -23.76478284628143456, -5.631829278076560641 ) ) ;
#7365 = CARTESIAN_POINT ( 'NONE',  ( 3.999999999999996447, -22.21612646813362346, -3.420118758496274225 ) ) ;
#7366 = CARTESIAN_POINT ( 'NONE',  ( -2.518350579753628526, 25.62180007765648426, -0.7558219633769075463 ) ) ;
#7367 = ORIENTED_EDGE ( 'NONE', *, *, #11282, .T. ) ;
#7368 = CARTESIAN_POINT ( 'NONE',  ( -1.135272562821090014, 18.49680007765648071, -3.311245368580554072 ) ) ;
#7369 = CARTESIAN_POINT ( 'NONE',  ( -5.577813053751546416E-15, -25.45076803941176991, -5.092196395636519490 ) ) ;
#7370 = DIRECTION ( 'NONE',  ( 0.000000000000000000, 0.000000000000000000, 1.000000000000000000 ) ) ;
#7371 = DIRECTION ( 'NONE',  ( 0.000000000000000000, 0.000000000000000000, 1.000000000000000000 ) ) ;
#7372 = CARTESIAN_POINT ( 'NONE',  ( 1.135272562821020070, 17.75319992234354771, -3.311245368580577164 ) ) ;
#7373 = ORIENTED_EDGE ( 'NONE', *, *, #16662, .T. ) ;
#7374 = CARTESIAN_POINT ( 'NONE',  ( 4.243569643750000786, -24.02932114822622722, -10.03594703378452024 ) ) ;
#7375 = AXIS2_PLACEMENT_3D ( 'NONE', #8238, #1209, #14167 ) ;
#7376 = CARTESIAN_POINT ( 'NONE',  ( 1.444289557196047680, 32.24680007765647360, 4.262301884875704161 ) ) ;
#7377 = VERTEX_POINT ( 'NONE', #10833 ) ;
#7378 = FACE_BOUND ( 'NONE', #6605, .T. ) ;
#7379 = DIRECTION ( 'NONE',  ( 0.000000000000000000, 1.000000000000000000, 0.000000000000000000 ) ) ;
#7380 = CARTESIAN_POINT ( 'NONE',  ( -5.330712181944245322E-15, -29.14017382041697601, -8.792020867043637722 ) ) ;
#7381 = CARTESIAN_POINT ( 'NONE',  ( -13.00000000000000178, 49.00000000000000000, 16.00000000000000000 ) ) ;
#7382 = CARTESIAN_POINT ( 'NONE',  ( 4.336808689942017736E-16, -0.7216878364870317197, 1.250000000000000000 ) ) ;
#7383 = LINE ( 'NONE', #9060, #214 ) ;
#7384 = CARTESIAN_POINT ( 'NONE',  ( 4.243569643750003451, -19.16166480309071574, -7.355703438614951573 ) ) ;
#7385 = EDGE_CURVE ( 'NONE', #4165, #17338, #9166, .T. ) ;
#7386 = ORIENTED_EDGE ( 'NONE', *, *, #5181, .F. ) ;
#7387 = EDGE_CURVE ( 'NONE', #3728, #278, #15026, .T. ) ;
#7388 = DIRECTION ( 'NONE',  ( -0.000000000000000000, -0.5735764363510414965, -0.8191520442889950182 ) ) ;
#7389 = CIRCLE ( 'NONE', #7995, 8.000000000000001776 ) ;
#7390 = LINE ( 'NONE', #8776, #9975 ) ;
#7391 = ADVANCED_FACE ( 'NONE', ( #15211, #5085 ), #9623, .T. ) ;
#7392 = EDGE_LOOP ( 'NONE', ( #11545, #2321, #11951, #38, #11570 ) ) ;
#7393 = EDGE_LOOP ( 'NONE', ( #5735, #7617, #15124, #2775 ) ) ;
#7394 = DIRECTION ( 'NONE',  ( -1.000000000000000000, 0.000000000000000000, 4.336808689942021680E-16 ) ) ;
#7395 = CARTESIAN_POINT ( 'NONE',  ( -9.000000000000001776, 16.59999999999999787, 2.499999999999998224 ) ) ;
#7396 = SURFACE_STYLE_FILL_AREA ( #13055 ) ;
#7397 = CARTESIAN_POINT ( 'NONE',  ( -3.673772985318163098, 26.75319992234354771, 2.599342558261029001 ) ) ;
#7398 = CARTESIAN_POINT ( 'NONE',  ( 2.115076519116425580, 31.12819992234354416, 3.012182706137062294 ) ) ;
#7399 = CARTESIAN_POINT ( 'NONE',  ( 1.593127413382998903, 39.62180007765647360, 2.091722143975139669 ) ) ;
#7400 = ORIENTED_EDGE ( 'NONE', *, *, #15392, .F. ) ;
#7401 = CARTESIAN_POINT ( 'NONE',  ( 4.518350579753602325, 30.62819992234354416, -1.405661355842793725 ) ) ;
#7402 = CARTESIAN_POINT ( 'NONE',  ( 4.000000000000003553, -19.61562664118283195, -7.758855928260364188 ) ) ;
#7403 = ORIENTED_EDGE ( 'NONE', *, *, #16258, .T. ) ;
#7404 = AXIS2_PLACEMENT_3D ( 'NONE', #13738, #2447, #3910 ) ;
#7405 = CARTESIAN_POINT ( 'NONE',  ( 1.820000000000000062, 0.000000000000000000, 0.000000000000000000 ) ) ;
#7406 = CARTESIAN_POINT ( 'NONE',  ( -3.481649420246369697, 30.37180007765647005, 1.193696214020542490 ) ) ;
#7407 =( BOUNDED_CURVE ( )  B_SPLINE_CURVE ( 2, ( #6400, #10477, #11864, #574, #11961, #7870, #7693, #2154, #846 ),
 .UNSPECIFIED., .F., .T. ) 
 B_SPLINE_CURVE_WITH_KNOTS ( ( 3, 2, 2, 2, 3 ),
 ( 0.06034482758620690612, 0.06321839080459770721, 0.06896551724137930939, 0.07471264367816092544, 0.07758620689655172653 ),
 .UNSPECIFIED. ) 
 CURVE ( )  GEOMETRIC_REPRESENTATION_ITEM ( )  RATIONAL_B_SPLINE_CURVE ( ( 0.9330127018922194093, 0.9330127018922195203, 1.000000000000000000, 0.8660254037844387076, 1.000000000000000000, 0.8660254037844387076, 1.000000000000000000, 0.9330127018922194093, 0.9330127018922194093 ) ) 
 REPRESENTATION_ITEM ( '' )  );
#7408 = CARTESIAN_POINT ( 'NONE',  ( -7.382399764659552943, -13.34693800548101095, 2.845224196420926610 ) ) ;
#7409 = CARTESIAN_POINT ( 'NONE',  ( 4.730628863548789710E-15, -17.33754842334290913, -9.022085378453862603 ) ) ;
#7410 = CARTESIAN_POINT ( 'NONE',  ( 4.499999999999999112, 31.74680007765647716, -0.05647727720537982360 ) ) ;
#7411 = LINE ( 'NONE', #1876, #6763 ) ;
#7412 = ORIENTED_EDGE ( 'NONE', *, *, #8820, .T. ) ;
#7413 = CARTESIAN_POINT ( 'NONE',  ( -3.481649420246369697, 27.87180007765647360, 1.193696214020542490 ) ) ;
#7414 = DIRECTION ( 'NONE',  ( 0.000000000000000000, 0.000000000000000000, -1.000000000000000000 ) ) ;
#7415 = CARTESIAN_POINT ( 'NONE',  ( -1.734723475976807094E-15, 38.59999999999999432, -2.500000000000000000 ) ) ;
#7416 = CARTESIAN_POINT ( 'NONE',  ( -4.000000000000007105, 6.938893903907228378E-15, 30.00000000000000000 ) ) ;
#7417 = SURFACE_SIDE_STYLE ('',( #6221 ) ) ;
#7418 = ORIENTED_EDGE ( 'NONE', *, *, #11882, .F. ) ;
#7419 = AXIS2_PLACEMENT_3D ( 'NONE', #11721, #12841, #3024 ) ;
#7420 = CARTESIAN_POINT ( 'NONE',  ( 3.481649420246394122, 28.37819992234354416, 1.193696214020467439 ) ) ;
#7421 = CARTESIAN_POINT ( 'NONE',  ( 1.300000000000000044, 0.7216878364870329410, -1.250000000000000000 ) ) ;
#7422 = CARTESIAN_POINT ( 'NONE',  ( -4.243569643750000786, -21.28690881192279960, -6.119376322027766157 ) ) ;
#7423 = CARTESIAN_POINT ( 'NONE',  ( -2.798362969681365886, 37.74680007765647360, 2.102939460078824929 ) ) ;
#7424 = EDGE_CURVE ( 'NONE', #12442, #10009, #17909, .T. ) ;
#7425 = CARTESIAN_POINT ( 'NONE',  ( -1.027846397803611866, 37.50319992234354061, -3.346150245485499219 ) ) ;
#7426 = CARTESIAN_POINT ( 'NONE',  ( -5.577813053751546416E-15, -23.12778347219005681, -1.774630616266089866 ) ) ;
#7427 = CARTESIAN_POINT ( 'NONE',  ( -5.279047395330986450E-15, -30.79721226948262824, -11.64886143429751542 ) ) ;
#7428 = CARTESIAN_POINT ( 'NONE',  ( 4.243569643750003451, -20.45221178488055713, -9.198795538265191141 ) ) ;
#7429 = CARTESIAN_POINT ( 'NONE',  ( 4.898587196589413815E-16, 2.700915433685006750, 35.11257424290206330 ) ) ;
#7430 = CARTESIAN_POINT ( 'NONE',  ( 8.000000000000000000, 18.79999999999999361, -2.500000000000000888 ) ) ;
#7431 = CARTESIAN_POINT ( 'NONE',  ( 0.000000000000000000, 15.00000000000000355, 0.000000000000000000 ) ) ;
#7432 = CARTESIAN_POINT ( 'NONE',  ( 1.300000000000000044, -1.443375672974064328, 1.278502688459867223E-18 ) ) ;
#7433 = ORIENTED_EDGE ( 'NONE', *, *, #12262, .F. ) ;
#7434 =( BOUNDED_CURVE ( )  B_SPLINE_CURVE ( 2, ( #12139, #10755, #3710, #9360, #7973, #13626, #938, #6582, #12233 ),
 .UNSPECIFIED., .F., .F. ) 
 B_SPLINE_CURVE_WITH_KNOTS ( ( 3, 2, 2, 2, 3 ),
 ( 0.5948275862068965747, 0.5977011494252874035, 0.6034482758620689502, 0.6091954022988506079, 0.6120689655172414367 ),
 .UNSPECIFIED. ) 
 CURVE ( )  GEOMETRIC_REPRESENTATION_ITEM ( )  RATIONAL_B_SPLINE_CURVE ( ( 0.9330127018922194093, 0.9330127018922194093, 1.000000000000000000, 0.8660254037844387076, 1.000000000000000000, 0.8660254037844387076, 1.000000000000000000, 0.9330127018922180770, 0.9330127018922194093 ) ) 
 REPRESENTATION_ITEM ( '' )  );
#7435 = EDGE_LOOP ( 'NONE', ( #16730, #5246, #7698, #8830, #12884 ) ) ;
#7436 = CARTESIAN_POINT ( 'NONE',  ( -4.243569643750000786, -19.73825243377498850, -3.907665802447479297 ) ) ;
#7437 = EDGE_CURVE ( 'NONE', #1761, #13129, #5319, .T. ) ;
#7438 = DIRECTION ( 'NONE',  ( -0.000000000000000000, -0.000000000000000000, -1.000000000000000000 ) ) ;
#7439 = CARTESIAN_POINT ( 'NONE',  ( 3.999999999999996447, -22.47423586449159671, -3.788737178426322849 ) ) ;
#7440 = ORIENTED_EDGE ( 'NONE', *, *, #16027, .T. ) ;
#7441 = TOROIDAL_SURFACE ( 'NONE', #8345, 9.000000000000001776, 0.9999999999999991118 ) ;
#7442 = CARTESIAN_POINT ( 'NONE',  ( 1.497042530366522461, 21.12819992234354416, 2.161531897785029965 ) ) ;
#7443 = EDGE_CURVE ( 'NONE', #1052, #10458, #2512, .T. ) ;
#7444 = CARTESIAN_POINT ( 'NONE',  ( -5.330712181944245322E-15, -29.62412893858816076, -9.483180404412477671 ) ) ;
#7445 = CARTESIAN_POINT ( 'NONE',  ( -2.211161402132902243, 15.87180007765647716, -2.942372952327172886 ) ) ;
#7446 =( GEOMETRIC_REPRESENTATION_CONTEXT ( 3 ) GLOBAL_UNCERTAINTY_ASSIGNED_CONTEXT ( ( #18290 ) ) GLOBAL_UNIT_ASSIGNED_CONTEXT ( ( #7674, #10364, #3146 ) ) REPRESENTATION_CONTEXT ( 'NONE', 'WORKASPACE' ) );
#7447 = LINE ( 'NONE', #3291, #4545 ) ;
#7448 = CARTESIAN_POINT ( 'NONE',  ( 7.649231854195297942, -10.00000000000000178, -6.849627928938597066 ) ) ;
#7449 = EDGE_LOOP ( 'NONE', ( #13796, #1636, #1188, #15944 ) ) ;
#7450 = CARTESIAN_POINT ( 'NONE',  ( 1.135272562821090458, 37.24680007765648071, 3.311245368580554072 ) ) ;
#7451 = CARTESIAN_POINT ( 'NONE',  ( -4.243569643750005227, -28.20868576974048025, -11.73320817580729880 ) ) ;
#7452 = VECTOR ( 'NONE', #11614, 1000.000000000000000 ) ;
#7453 = CARTESIAN_POINT ( 'NONE',  ( -1.734723475976807094E-15, 20.99999999999999289, -2.500000000000000000 ) ) ;
#7454 = MECHANICAL_DESIGN_GEOMETRIC_PRESENTATION_REPRESENTATION (  '', ( #2168 ), #5969 ) ;
#7455 = CARTESIAN_POINT ( 'NONE',  ( 4.243569643750000786, -26.06193264454523018, -12.93881709073364661 ) ) ;
#7456 = CARTESIAN_POINT ( 'NONE',  ( 9.000000000000005329, 25.39999999999999503, 2.499999999999997335 ) ) ;
#7457 = DIRECTION ( 'NONE',  ( 0.000000000000000000, 0.000000000000000000, -1.000000000000000000 ) ) ;
#7458 = DIRECTION ( 'NONE',  ( -0.000000000000000000, 1.000000000000000000, -0.000000000000000000 ) ) ;
#7459 = CARTESIAN_POINT ( 'NONE',  ( -2.121784821875005722, -27.86783793146007326, -9.110681959144070419 ) ) ;
#7460 = DIRECTION ( 'NONE',  ( -4.915049848600951133E-16, 0.000000000000000000, -1.000000000000000000 ) ) ;
#7461 = CARTESIAN_POINT ( 'NONE',  ( -4.000000000000000888, -20.17381204048153265, -4.529709386582819519 ) ) ;
#7462 = CARTESIAN_POINT ( 'NONE',  ( 2.055738996568313048, 24.49680007765648426, 1.423772053676023441 ) ) ;
#7463 = ADVANCED_FACE ( 'NONE', ( #6749 ), #16788, .F. ) ;
#7464 = VERTEX_POINT ( 'NONE', #16696 ) ;
#7465 = CARTESIAN_POINT ( 'NONE',  ( -1.135272562821090014, 23.49680007765647716, -3.311245368580554072 ) ) ;
#7466 = DIRECTION ( 'NONE',  ( 1.000000000000000000, 0.000000000000000000, 0.000000000000000000 ) ) ;
#7467 = CARTESIAN_POINT ( 'NONE',  ( 2.000000000000004441, -23.10062930614460797, -14.74911449125581520 ) ) ;
#7468 = AXIS2_PLACEMENT_3D ( 'NONE', #14362, #4257, #2702 ) ;
#7469 = CYLINDRICAL_SURFACE ( 'NONE', #11336, 4.000000000000000888 ) ;
#7470 = CARTESIAN_POINT ( 'NONE',  ( 3.518350579753605434, 20.62819992234354771, -1.080741659609877114 ) ) ;
#7471 = EDGE_LOOP ( 'NONE', ( #3381, #16000, #10596, #6340 ) ) ;
#7472 = CARTESIAN_POINT ( 'NONE',  ( 4.243569643750003451, -22.51708695574430763, -12.14774289770557303 ) ) ;
#7473 = CARTESIAN_POINT ( 'NONE',  ( -2.829195390882805139, 38.37180007765647360, -3.793023760679206102 ) ) ;
#7474 = ORIENTED_EDGE ( 'NONE', *, *, #8857, .T. ) ;
#7475 = CARTESIAN_POINT ( 'NONE',  ( -4.000000000000000888, -22.49679660770325285, -7.847275165953248255 ) ) ;
#7476 = CARTESIAN_POINT ( 'NONE',  ( 2.121784821874994176, -28.63141156235240459, -10.20117811810379216 ) ) ;
#7477 = DIRECTION ( 'NONE',  ( 0.000000000000000000, 0.000000000000000000, -1.000000000000000000 ) ) ;
#7478 = CIRCLE ( 'NONE', #11932, 10.00000000000000000 ) ;
#7479 = DIRECTION ( 'NONE',  ( -0.000000000000000000, -1.000000000000000000, -0.000000000000000000 ) ) ;
#7480 = CIRCLE ( 'NONE', #1282, 10.00000000000000000 ) ;
#7481 = CARTESIAN_POINT ( 'NONE',  ( 4.000000000000000888, -22.56132395608780783, -7.939429769928989522 ) ) ;
#7482 = CARTESIAN_POINT ( 'NONE',  ( 4.243569643749996345, -23.47668016984439632, -4.975203810423082906 ) ) ;
#7483 = EDGE_LOOP ( 'NONE', ( #4599, #8010, #14111, #14680 ) ) ;
#7484 = DIRECTION ( 'NONE',  ( 0.000000000000000000, 0.000000000000000000, 1.000000000000000000 ) ) ;
#7485 = CARTESIAN_POINT ( 'NONE',  ( 0.000000000000000000, 5.977523610840987267, 32.81826849749789687 ) ) ;
#7486 = CARTESIAN_POINT ( 'NONE',  ( -10.00000000000000000, 31.99999999999999289, 2.499999999999998224 ) ) ;
#7487 = ORIENTED_EDGE ( 'NONE', *, *, #2747, .T. ) ;
#7488 = EDGE_LOOP ( 'NONE', ( #6238, #17361, #9256, #4487 ) ) ;
#7489 = CARTESIAN_POINT ( 'NONE',  ( 1.071796769724495224, -20.84489885850341651, -12.46190787057612681 ) ) ;
#7490 = DIRECTION ( 'NONE',  ( 0.9454169814551708351, 0.000000000000000000, 0.3258630558627246820 ) ) ;
#7491 = CARTESIAN_POINT ( 'NONE',  ( -1.444289557195956863, 26.50319992234354771, 4.262301884875733471 ) ) ;
#7492 = CARTESIAN_POINT ( 'NONE',  ( -1.027846397803611866, 30.00319992234354416, -3.346150245485499219 ) ) ;
#7493 = CARTESIAN_POINT ( 'NONE',  ( -1.593127413382952939, 19.12819992234354771, 2.091722143975172532 ) ) ;
#7494 = VERTEX_POINT ( 'NONE', #15299 ) ;
#7495 = CARTESIAN_POINT ( 'NONE',  ( 2.733110507866328920, 38.62819992234354771, 3.862833514489095510 ) ) ;
#7496 = CARTESIAN_POINT ( 'NONE',  ( 3.999999999999996447, -23.70025549648700292, -5.539674672087284257 ) ) ;
#7497 = EDGE_LOOP ( 'NONE', ( #5163, #1032, #16389, #17075 ) ) ;
#7498 = EDGE_CURVE ( 'NONE', #11197, #17312, #8323, .T. ) ;
#7499 = DIRECTION ( 'NONE',  ( 0.000000000000000000, 0.000000000000000000, -1.000000000000000000 ) ) ;
#7500 = EDGE_CURVE ( 'NONE', #10864, #9690, #14824, .T. ) ;
#7501 = CARTESIAN_POINT ( 'NONE',  ( -1.027846397803541700, 29.99680007765648071, 3.346150245485522312 ) ) ;
#7502 = PLANE ( 'NONE',  #11652 ) ;
#7503 = EDGE_CURVE ( 'NONE', #2915, #6628, #13320, .T. ) ;
#7504 = CARTESIAN_POINT ( 'NONE',  ( 4.243569643750003451, -19.12940112854596819, -7.309626136123695161 ) ) ;
#7505 = CARTESIAN_POINT ( 'NONE',  ( -4.518350579753632523, 30.62180007765647005, -1.405661355842698468 ) ) ;
#7506 = TOROIDAL_SURFACE ( 'NONE', #2505, 9.000000000000001776, 0.9999999999999991118 ) ;
#7507 = PRODUCT_DEFINITION_SHAPE ( 'NONE', 'NONE',  #12171 ) ;
#7508 = EDGE_CURVE ( 'NONE', #2199, #11229, #7082, .T. ) ;
#7509 = FACE_BOUND ( 'NONE', #5526, .T. ) ;
#7510 = ORIENTED_EDGE ( 'NONE', *, *, #131, .F. ) ;
#7511 = CARTESIAN_POINT ( 'NONE',  ( 3.500000000000000444, 29.24680007765647716, -0.05647727720536935281 ) ) ;
#7512 = COLOUR_RGB ( '',1.000000000000000000, 0.9490196078431372140, 0.9098039215686274384 ) ;
#7513 = CARTESIAN_POINT ( 'NONE',  ( -1.071796769724496334, -26.43020497576804217, -6.490977304023350491 ) ) ;
#7514 = CARTESIAN_POINT ( 'NONE',  ( -8.000000000000000000, 46.00000000000000000, 2.499999999999999112 ) ) ;
#7515 = CARTESIAN_POINT ( 'NONE',  ( 1.300000000000000044, -0.7216878364870317197, -1.250000000000000000 ) ) ;
#7516 = ORIENTED_EDGE ( 'NONE', *, *, #17101, .F. ) ;
#7517 = CARTESIAN_POINT ( 'NONE',  ( -2.211161402132839182, 24.12819992234354416, 2.942372952327218627 ) ) ;
#7518 = LINE ( 'NONE', #3362, #3942 ) ;
#7519 = CARTESIAN_POINT ( 'NONE',  ( 4.243569643750003451, -18.87129173218799849, -6.941007716193646537 ) ) ;
#7520 = CARTESIAN_POINT ( 'NONE',  ( -0.7188294034286043521, 22.49680007765648071, 2.395093729190366005 ) ) ;
#7521 = ADVANCED_FACE ( 'NONE', ( #15391 ), #2691, .F. ) ;
#7522 = CARTESIAN_POINT ( 'NONE',  ( 3.481649420246394122, 33.37819992234353350, 1.193696214020467439 ) ) ;
#7523 = LINE ( 'NONE', #16163, #17366 ) ;
#7524 = CARTESIAN_POINT ( 'NONE',  ( 3.999999999999996447, -28.34622463093043621, -12.17480623082814262 ) ) ;
#7525 =( BOUNDED_CURVE ( )  B_SPLINE_CURVE ( 2, ( #11542, #2942, #5719, #11359, #17048, #4320, #10150, #8577, #3125 ),
 .UNSPECIFIED., .F., .F. ) 
 B_SPLINE_CURVE_WITH_KNOTS ( ( 3, 2, 2, 2, 3 ),
 ( 0.5258620689655172376, 0.5287356321839080664, 0.5344827586206896131, 0.5402298850574712707, 0.5431034482758620996 ),
 .UNSPECIFIED. ) 
 CURVE ( )  GEOMETRIC_REPRESENTATION_ITEM ( )  RATIONAL_B_SPLINE_CURVE ( ( 0.9330127018922194093, 0.9330127018922194093, 1.000000000000000000, 0.8660254037844387076, 1.000000000000000000, 0.8660254037844387076, 1.000000000000000000, 0.9330127018922194093, 0.9330127018922194093 ) ) 
 REPRESENTATION_ITEM ( '' )  );
#7526 = CARTESIAN_POINT ( 'NONE',  ( 4.730628863548789710E-15, -17.88603089060359963, -9.805399520805213598 ) ) ;
#7527 = CYLINDRICAL_SURFACE ( 'NONE', #640, 4.000000000000000000 ) ;
#7528 = CARTESIAN_POINT ( 'NONE',  ( 0.000000000000000000, 31.99999999999999289, 2.500000000000000000 ) ) ;
#7529 = CARTESIAN_POINT ( 'NONE',  ( -8.999999999999996447, -10.00000000000000000, 30.00000000000000000 ) ) ;
#7530 = DIRECTION ( 'NONE',  ( -4.915049848600951133E-16, 0.000000000000000000, -1.000000000000000000 ) ) ;
#7531 = ORIENTED_EDGE ( 'NONE', *, *, #14532, .T. ) ;
#7532 = ORIENTED_EDGE ( 'NONE', *, *, #17898, .T. ) ;
#7533 = SURFACE_SIDE_STYLE ('',( #14600 ) ) ;
#7534 = CARTESIAN_POINT ( 'NONE',  ( 9.000000000000001776, 43.00000000000000000, -2.500000000000002665 ) ) ;
#7535 = PLANE ( 'NONE',  #1140 ) ;
#7536 = ORIENTED_EDGE ( 'NONE', *, *, #4113, .F. ) ;
#7537 = CARTESIAN_POINT ( 'NONE',  ( 0.05938372350921204690, 30.12819992234354416, -2.628655560595669183 ) ) ;
#7538 = CARTESIAN_POINT ( 'NONE',  ( -4.243569643750000786, -25.67476855000827030, -12.38588946083857856 ) ) ;
#7539 = CARTESIAN_POINT ( 'NONE',  ( 2.115076519116362963, 26.37180007765648071, -3.012182706137107147 ) ) ;
#7540 = FACE_OUTER_BOUND ( 'NONE', #10210, .T. ) ;
#7541 = CARTESIAN_POINT ( 'NONE',  ( 5.940121053391558270, -10.00000000000000178, -9.400027718824636835 ) ) ;
#7542 = ORIENTED_EDGE ( 'NONE', *, *, #1117, .T. ) ;
#7543 = CARTESIAN_POINT ( 'NONE',  ( 0.05938372350927906274, 39.87180007765648071, 3.680117784833935701 ) ) ;
#7544 = CARTESIAN_POINT ( 'NONE',  ( 3.999999999999996447, -21.89348972198121857, -2.959345732576948773 ) ) ;
#7545 = CARTESIAN_POINT ( 'NONE',  ( -3.999999999999997335, -23.20764907453616743, -12.88879560662696200 ) ) ;
#7546 = CARTESIAN_POINT ( 'NONE',  ( 2.121784821874994176, -27.82481969873374794, -9.049245555822391651 ) ) ;
#7547 = DIRECTION ( 'NONE',  ( 0.000000000000000000, 0.000000000000000000, 1.000000000000000000 ) ) ;
#7548 = CARTESIAN_POINT ( 'NONE',  ( 1.300000000000000044, -0.7216878364870317197, -1.250000000000000000 ) ) ;
#7549 = CARTESIAN_POINT ( 'NONE',  ( 8.499999999999994671, 13.00000000000000000, 20.49999999999999645 ) ) ;
#7550 = CARTESIAN_POINT ( 'NONE',  ( -5.330712181944245322E-15, -27.30114437136644767, -6.165614625042047159 ) ) ;
#7551 = CARTESIAN_POINT ( 'NONE',  ( -8.000000000000001776, 34.19999999999999574, 2.499999999999995115 ) ) ;
#7552 = CARTESIAN_POINT ( 'NONE',  ( 9.000000000000001776, 27.59999999999999432, -2.500000000000002665 ) ) ;
#7553 = CARTESIAN_POINT ( 'NONE',  ( -0.05938372350926768989, 31.12180007765648426, -2.628655560595669183 ) ) ;
#7554 = ORIENTED_EDGE ( 'NONE', *, *, #13117, .F. ) ;
#7555 = CARTESIAN_POINT ( 'NONE',  ( -1.027846397803541700, 24.99680007765647716, 3.346150245485522312 ) ) ;
#7556 = DIRECTION ( 'NONE',  ( 0.000000000000000000, 0.000000000000000000, 1.000000000000000000 ) ) ;
#7557 = CARTESIAN_POINT ( 'NONE',  ( 4.000000000000003553, -23.55179493634680199, -13.38028683320035483 ) ) ;
#7558 = CARTESIAN_POINT ( 'NONE',  ( 4.898587196589413815E-16, 2.700915433685006750, 35.11257424290206330 ) ) ;
#7559 = CARTESIAN_POINT ( 'NONE',  ( 2.115076519116426024, 18.62819992234354771, 3.012182706137062294 ) ) ;
#7560 = ORIENTED_EDGE ( 'NONE', *, *, #18194, .F. ) ;
#7561 = CARTESIAN_POINT ( 'NONE',  ( 4.730628863548789710E-15, -19.43468726875141073, -12.01711004038550001 ) ) ;
#7562 = CARTESIAN_POINT ( 'NONE',  ( 3.481649420246369697, 16.62180007765648071, -1.193696214020541824 ) ) ;
#7563 = ORIENTED_EDGE ( 'NONE', *, *, #10366, .F. ) ;
#7564 = AXIS2_PLACEMENT_3D ( 'NONE', #11136, #1418, #14107 ) ;
#7565 = CARTESIAN_POINT ( 'NONE',  ( -4.648177544792955347E-16, -29.83862777749724060, -11.35870953444733011 ) ) ;
#7566 = ADVANCED_FACE ( 'NONE', ( #1648 ), #10159, .F. ) ;
#7567 = CARTESIAN_POINT ( 'NONE',  ( 0.000000000000000000, 40.79999999999999716, 2.500000000000000000 ) ) ;
#7568 = VECTOR ( 'NONE', #14280, 1000.000000000000000 ) ;
#7569 = CARTESIAN_POINT ( 'NONE',  ( 4.243569643750000786, -26.09419631908997772, -12.98489439322490213 ) ) ;
#7570 = CARTESIAN_POINT ( 'NONE',  ( 1.071796769724495224, -23.36146547228866410, -16.05593746388732868 ) ) ;
#7571 = CARTESIAN_POINT ( 'NONE',  ( -3.999999999999997335, -23.98197726361007298, -13.99465086641710698 ) ) ;
#7572 = CARTESIAN_POINT ( 'NONE',  ( 4.299564228933482956E-15, -19.22018842984233089, -10.14158091035064579 ) ) ;
#7573 = CARTESIAN_POINT ( 'NONE',  ( -4.243569643750000786, -20.54484429739364515, -5.059598364728879361 ) ) ;
#7574 = VERTEX_POINT ( 'NONE', #2950 ) ;
#7575 = CARTESIAN_POINT ( 'NONE',  ( -1.734723475976807094E-15, 34.19999999999999574, -2.500000000000000000 ) ) ;
#7576 = CARTESIAN_POINT ( 'NONE',  ( 1.999999999999994449, -25.76460485463143968, -6.474712139601389360 ) ) ;
#7577 = CARTESIAN_POINT ( 'NONE',  ( -8.500000000000010658, 15.00000000000000000, 22.69999999999999218 ) ) ;
#7578 = ORIENTED_EDGE ( 'NONE', *, *, #17316, .F. ) ;
#7579 = ORIENTED_EDGE ( 'NONE', *, *, #8820, .F. ) ;
#7580 = DIRECTION ( 'NONE',  ( 0.000000000000000000, 0.000000000000000000, -1.000000000000000000 ) ) ;
#7581 = CARTESIAN_POINT ( 'NONE',  ( -14.99999999999999645, -10.00000000000000000, 30.00000000000000000 ) ) ;
#7582 = CARTESIAN_POINT ( 'NONE',  ( -2.733110507866328476, 22.37819992234354416, -3.862833514489096398 ) ) ;
#7583 = CARTESIAN_POINT ( 'NONE',  ( -3.518350579753606322, 36.87819992234354061, 1.080741659609877781 ) ) ;
#7584 = CARTESIAN_POINT ( 'NONE',  ( -0.7188294034286550893, 22.50319992234354771, -2.395093729190349130 ) ) ;
#7585 = ORIENTED_EDGE ( 'NONE', *, *, #14666, .T. ) ;
#7586 = CARTESIAN_POINT ( 'NONE',  ( -2.829195390882724315, 39.12819992234354771, 3.793023760679264722 ) ) ;
#7587 = CARTESIAN_POINT ( 'NONE',  ( -5.279047395330986450E-15, -25.63502434232325911, -4.276493035696559808 ) ) ;
#7588 = VERTEX_POINT ( 'NONE', #8489 ) ;
#7589 = CARTESIAN_POINT ( 'NONE',  ( 4.898587196589413815E-16, 2.700915433685006750, 35.11257424290206330 ) ) ;
#7590 = CARTESIAN_POINT ( 'NONE',  ( -1.135272562821090014, 28.49680007765648071, -3.311245368580554072 ) ) ;
#7591 = DIRECTION ( 'NONE',  ( -0.000000000000000000, 1.000000000000000000, -0.000000000000000000 ) ) ;
#7592 =( REPRESENTATION_RELATIONSHIP ('NONE','NONE', #15868, #10877 ) REPRESENTATION_RELATIONSHIP_WITH_TRANSFORMATION ( #8109 )SHAPE_REPRESENTATION_RELATIONSHIP( ) );
#7593 = CARTESIAN_POINT ( 'NONE',  ( -5.330712181944246111E-15, -24.97815980414473103, -2.848048845671618423 ) ) ;
#7594 = AXIS2_PLACEMENT_3D ( 'NONE', #17669, #6332, #863 ) ;
#7595 = CARTESIAN_POINT ( 'NONE',  ( 0.05938372350929014415, 27.37180007765647716, 4.731580009072201776 ) ) ;
#7596 = CARTESIAN_POINT ( 'NONE',  ( -3.999999999999997335, -21.07824655387798174, -9.847693641197304615 ) ) ;
#7597 = ORIENTED_EDGE ( 'NONE', *, *, #8491, .T. ) ;
#7598 = CARTESIAN_POINT ( 'NONE',  ( 2.798362969681366330, 33.99680007765648071, -2.102939460078824929 ) ) ;
#7599 = CARTESIAN_POINT ( 'NONE',  ( -1.801903668194536401, -10.00000000000000178, 23.81845480839542972 ) ) ;
#7600 = EDGE_CURVE ( 'NONE', #18352, #8879, #3036, .T. ) ;
#7601 = FACE_OUTER_BOUND ( 'NONE', #14468, .T. ) ;
#7602 = ORIENTED_EDGE ( 'NONE', *, *, #1845, .T. ) ;
#7603 = CARTESIAN_POINT ( 'NONE',  ( 3.518350579753605434, 25.62819992234353705, -1.080741659609877114 ) ) ;
#7604 = ADVANCED_FACE ( 'NONE', ( #4421 ), #4154, .F. ) ;
#7605 = FACE_BOUND ( 'NONE', #15364, .T. ) ;
#7606 = CARTESIAN_POINT ( 'NONE',  ( -2.121784821875005722, -24.25430638244851167, -3.950024080123402559 ) ) ;
#7607 = CARTESIAN_POINT ( 'NONE',  ( -2.500000000000001332, 22.99680007765648071, 0.05647727720535858364 ) ) ;
#7608 = CARTESIAN_POINT ( 'NONE',  ( 2.733110507866328920, 16.12819992234354416, 3.862833514489095510 ) ) ;
#7609 = CARTESIAN_POINT ( 'NONE',  ( 3.999999999999996447, -21.69990767541768761, -2.682881918636179197 ) ) ;
#7610 = CIRCLE ( 'NONE', #17720, 8.000000000000000000 ) ;
#7611 = CARTESIAN_POINT ( 'NONE',  ( -1.999999999999996225, -22.73497432726586709, -14.22690506201481853 ) ) ;
#7612 = CARTESIAN_POINT ( 'NONE',  ( 4.730628863548789710E-15, -17.11170270152969053, -8.699544261015072166 ) ) ;
#7613 = CARTESIAN_POINT ( 'NONE',  ( 3.250767888004682415, -21.90484815091188509, -2.246271217071878823 ) ) ;
#7614 = CARTESIAN_POINT ( 'NONE',  ( -4.000000000000000888, -25.52958201420443984, -12.17854159912454293 ) ) ;
#7615 = VECTOR ( 'NONE', #17442, 1000.000000000000000 ) ;
#7616 = CYLINDRICAL_SURFACE ( 'NONE', #4979, 0.9999999999999991118 ) ;
#7617 = ORIENTED_EDGE ( 'NONE', *, *, #4884, .F. ) ;
#7618 = AXIS2_PLACEMENT_3D ( 'NONE', #7734, #887, #16657 ) ;
#7619 = EDGE_LOOP ( 'NONE', ( #8043, #12753, #6936, #17726 ) ) ;
#7620 = CARTESIAN_POINT ( 'NONE',  ( 3.579096709490575479E-14, -22.86967407583208711, -1.406012196336041020 ) ) ;
#7621 = DIRECTION ( 'NONE',  ( -1.000000000000000000, 0.000000000000000000, 0.000000000000000000 ) ) ;
#7622 = FILL_AREA_STYLE ('',( #4852 ) ) ;
#7623 = ORIENTED_EDGE ( 'NONE', *, *, #3500, .T. ) ;
#7624 = CARTESIAN_POINT ( 'NONE',  ( 0.7188294034286553114, 28.75319992234354771, 2.395093729190349130 ) ) ;
#7625 = EDGE_CURVE ( 'NONE', #7076, #3912, #4431, .T. ) ;
#7626 = CARTESIAN_POINT ( 'NONE',  ( 4.243569643749996345, -27.05794804431121037, -10.08978438695249835 ) ) ;
#7627 = CARTESIAN_POINT ( 'NONE',  ( 2.864755990943265829, 24.49680007765647716, 2.011557305968487697 ) ) ;
#7628 =( BOUNDED_CURVE ( )  B_SPLINE_CURVE ( 2, ( #10479, #9542, #9718, #5376, #3982, #13812, #13993, #12415, #15219 ),
 .UNSPECIFIED., .F., .T. ) 
 B_SPLINE_CURVE_WITH_KNOTS ( ( 3, 2, 2, 2, 3 ),
 ( 0.2672413793103448620, 0.2701149425287356354, 0.2758620689655172376, 0.2816091954022988397, 0.2844827586206896686 ),
 .UNSPECIFIED. ) 
 CURVE ( )  GEOMETRIC_REPRESENTATION_ITEM ( )  RATIONAL_B_SPLINE_CURVE ( ( 0.9330127018922194093, 0.9330127018922200755, 1.000000000000000000, 0.8660254037844387076, 1.000000000000000000, 0.8660254037844387076, 1.000000000000000000, 0.9330127018922187432, 0.9330127018922194093 ) ) 
 REPRESENTATION_ITEM ( '' )  );
#7629 = DIRECTION ( 'NONE',  ( -0.000000000000000000, -0.5735764363510414965, -0.8191520442889950182 ) ) ;
#7630 = DIRECTION ( 'NONE',  ( -0.000000000000000000, -1.000000000000000000, -0.000000000000000000 ) ) ;
#7631 = CLOSED_SHELL ( 'NONE', ( #17170, #17395, #1509, #2873, #13560, #10893, #17839, #13477, #16610, #5751 ) ) ;
#7632 = AXIS2_PLACEMENT_3D ( 'NONE', #6425, #8085, #15060 ) ;
#7633 = CARTESIAN_POINT ( 'NONE',  ( 4.243569643750003451, -22.77519635210228088, -12.51636131763562076 ) ) ;
#7634 = VECTOR ( 'NONE', #5116, 1000.000000000000000 ) ;
#7635 = DIRECTION ( 'NONE',  ( 0.000000000000000000, 1.000000000000000000, 0.000000000000000000 ) ) ;
#7636 = CARTESIAN_POINT ( 'NONE',  ( -4.243569643750004339, -26.36965632068995191, -9.106801933805707350 ) ) ;
#7637 = CYLINDRICAL_SURFACE ( 'NONE', #17082, 4.000000000000000000 ) ;
#7638 = DIRECTION ( 'NONE',  ( -0.000000000000000000, -0.5735764363510414965, -0.8191520442889950182 ) ) ;
#7639 = CYLINDRICAL_SURFACE ( 'NONE', #16543, 6.500000000000000000 ) ;
#7640 = CARTESIAN_POINT ( 'NONE',  ( -2.121784821874996396, -20.64249580861881128, -11.60629434330255982 ) ) ;
#7641 = CYLINDRICAL_SURFACE ( 'NONE', #7132, 2.149999999999995470 ) ;
#7642 = CARTESIAN_POINT ( 'NONE',  ( -5.279047395330986450E-15, -23.37656712489597410, -1.051081862315407234 ) ) ;
#7643 = CARTESIAN_POINT ( 'NONE',  ( 0.8262555684461332373, 29.74680007765648426, 2.360188852285403982 ) ) ;
#7644 = CIRCLE ( 'NONE', #14483, 8.000000000000003553 ) ;
#7645 = EDGE_LOOP ( 'NONE', ( #1741, #6222, #10732, #4513 ) ) ;
#7646 = CARTESIAN_POINT ( 'NONE',  ( -1.135272562821090014, 30.99680007765647716, -3.311245368580554072 ) ) ;
#7647 = CARTESIAN_POINT ( 'NONE',  ( 2.000000000000004441, -21.55197292799679687, -12.53740397167552878 ) ) ;
#7648 = CARTESIAN_POINT ( 'NONE',  ( 3.579096709490575479E-14, -23.64400226490599266, -2.511867456126184894 ) ) ;
#7649 = CARTESIAN_POINT ( 'NONE',  ( 1.135272562821020070, 15.25319992234354594, -3.311245368580577164 ) ) ;
#7650 = EDGE_LOOP ( 'NONE', ( #719, #1368, #4733, #12066 ) ) ;
#7651 = CARTESIAN_POINT ( 'NONE',  ( 4.243569643750003451, -20.71032118123852683, -9.567413958195238877 ) ) ;
#7652 = CARTESIAN_POINT ( 'NONE',  ( -3.607379964056306676, 40.24680007765648071, 2.690724712371306282 ) ) ;
#7653 = ORIENTED_EDGE ( 'NONE', *, *, #1404, .T. ) ;
#7654 = AXIS2_PLACEMENT_3D ( 'NONE', #11101, #4329, #445 ) ;
#7655 = CYLINDRICAL_SURFACE ( 'NONE', #12104, 2.149999999999995470 ) ;
#7656 = CARTESIAN_POINT ( 'NONE',  ( -4.243569643750000786, -24.93270403547910874, -11.32611150353969087 ) ) ;
#7657 = LINE ( 'NONE', #17433, #5208 ) ;
#7658 = CARTESIAN_POINT ( 'NONE',  ( 9.849679380115679450, -9.940103771709287273, 9.708927138098026433 ) ) ;
#7659 = DIRECTION ( 'NONE',  ( -0.000000000000000000, 1.000000000000000000, -0.000000000000000000 ) ) ;
#7660 = CARTESIAN_POINT ( 'NONE',  ( -4.243569643750000786, -20.28673490103567545, -4.690979944798832513 ) ) ;
#7661 = ORIENTED_EDGE ( 'NONE', *, *, #11348, .F. ) ;
#7662 = CARTESIAN_POINT ( 'NONE',  ( -4.000000000000004441, -21.78594414087033471, -2.805754725279534956 ) ) ;
#7663 = VECTOR ( 'NONE', #2926, 1000.000000000000114 ) ;
#7664 = ADVANCED_FACE ( 'NONE', ( #4247 ), #9889, .F. ) ;
#7665 = CARTESIAN_POINT ( 'NONE',  ( -2.000000000000005773, -26.06573248371572760, -6.904766962853115864 ) ) ;
#7666 = AXIS2_PLACEMENT_3D ( 'NONE', #8289, #8194, #9767 ) ;
#7667 = CARTESIAN_POINT ( 'NONE',  ( -2.465190328815646976E-33, -26.97786251599082519, -14.24690051095425858 ) ) ;
#7668 = EDGE_LOOP ( 'NONE', ( #3776, #7892, #9968, #15739 ) ) ;
#7669 = ORIENTED_EDGE ( 'NONE', *, *, #844, .F. ) ;
#7670 = CARTESIAN_POINT ( 'NONE',  ( 4.000000000000000000, 0.000000000000000000, 3.047499999999999876 ) ) ;
#7671 = EDGE_CURVE ( 'NONE', #4080, #3700, #4729, .T. ) ;
#7672 = MANIFOLD_SOLID_BREP ( 'Sweep1', #7922 ) ;
#7673 = CARTESIAN_POINT ( 'NONE',  ( 0.000000000000000000, 20.99999999999999289, 2.500000000000000000 ) ) ;
#7674 =( LENGTH_UNIT ( ) NAMED_UNIT ( * ) SI_UNIT ( .MILLI., .METRE. ) );
#7675 = AXIS2_PLACEMENT_3D ( 'NONE', #12019, #3684, #11933 ) ;
#7676 = CARTESIAN_POINT ( 'NONE',  ( 4.481649420246397675, 28.37819992234355126, 1.518615910253363177 ) ) ;
#7677 = CARTESIAN_POINT ( 'NONE',  ( 2.864755990943222308, 35.50319992234354771, -2.011557305968548093 ) ) ;
#7679 = EDGE_CURVE ( 'NONE', #894, #3649, #15119, .T. ) ;
#7678 = VECTOR ( 'NONE', #8232, 1000.000000000000000 ) ;
#7680 = CARTESIAN_POINT ( 'NONE',  ( 0.7188294034286553114, 23.75319992234354771, 2.395093729190349130 ) ) ;
#7681 = ORIENTED_EDGE ( 'NONE', *, *, #9909, .F. ) ;
#7682 = CARTESIAN_POINT ( 'NONE',  ( 4.481649420246397675, 38.37819992234354061, 1.518615910253363177 ) ) ;
#7683 = CARTESIAN_POINT ( 'NONE',  ( 1.999999999999994449, -24.66763991940512568, -4.908083853891920256 ) ) ;
#7684 = SHAPE_REPRESENTATION ( 'coil', ( #16940 ), #11010 ) ;
#7685 = ORIENTED_EDGE ( 'NONE', *, *, #2931, .T. ) ;
#7686 = LINE ( 'NONE', #10275, #16278 ) ;
#7687 = CARTESIAN_POINT ( 'NONE',  ( 3.500000000000000444, 34.24680007765648071, -0.05647727720536935281 ) ) ;
#7688 = LINE ( 'NONE', #17650, #7180 ) ;
#7689 = AXIS2_PLACEMENT_3D ( 'NONE', #7548, #10232, #11349 ) ;
#7690 = CARTESIAN_POINT ( 'NONE',  ( -4.243569643750004339, -21.98179658260448832, -2.840288794994898058 ) ) ;
#7691 = AXIS2_PLACEMENT_3D ( 'NONE', #16877, #12944, #14348 ) ;
#7692 = CARTESIAN_POINT ( 'NONE',  ( 4.243569643750000786, -23.51310235551028782, -9.298710193924424772 ) ) ;
#7693 = CARTESIAN_POINT ( 'NONE',  ( 2.000000000000004441, -23.61684809886054381, -15.48635133111591067 ) ) ;
#7694 = ORIENTED_EDGE ( 'NONE', *, *, #9322, .T. ) ;
#7695 = FACE_OUTER_BOUND ( 'NONE', #13374, .T. ) ;
#7696 = DIRECTION ( 'NONE',  ( 1.000000000000000000, 0.000000000000000000, 0.000000000000000000 ) ) ;
#7697 = CARTESIAN_POINT ( 'NONE',  ( 4.730628863548789710E-15, -22.79010942140500262, -16.80914949947612413 ) ) ;
#7698 = ORIENTED_EDGE ( 'NONE', *, *, #6896, .T. ) ;
#7699 = CARTESIAN_POINT ( 'NONE',  ( 1.027846397803612311, 28.75319992234354416, 3.346150245485499219 ) ) ;
#7700 = CARTESIAN_POINT ( 'NONE',  ( 3.518350579753606322, 15.62819992234354416, -1.080741659609876892 ) ) ;
#7701 = CARTESIAN_POINT ( 'NONE',  ( -4.243569643750005227, -23.78856235711026912, -5.420617734505229990 ) ) ;
#7702 = CARTESIAN_POINT ( 'NONE',  ( -2.481649420246374138, 20.37180007765648426, 0.8687765177876256573 ) ) ;
#7703 = AXIS2_PLACEMENT_3D ( 'NONE', #3373, #14595, #2082 ) ;
#7704 = CARTESIAN_POINT ( 'NONE',  ( -3.607379964056363075, 17.25319992234354416, -2.690724712371229899 ) ) ;
#7705 = CARTESIAN_POINT ( 'NONE',  ( 2.121784821874994176, -29.40573975142631014, -11.30703337789393359 ) ) ;
#7706 = CARTESIAN_POINT ( 'NONE',  ( -4.000000000000000888, -26.30391020327834539, -13.28439685891468613 ) ) ;
#7707 = MANIFOLD_SOLID_BREP ( 'LPattern6[2]', #15343 ) ;
#7708 = CARTESIAN_POINT ( 'NONE',  ( 2.121784821874994176, -24.75977061698287329, -4.671901819153075230 ) ) ;
#7709 = CARTESIAN_POINT ( 'NONE',  ( 3.607379964056306676, 38.99680007765648071, -2.690724712371305838 ) ) ;
#7710 = EDGE_CURVE ( 'NONE', #1376, #1446, #11543, .T. ) ;
#7711 = CARTESIAN_POINT ( 'NONE',  ( -6.158835246850665095E-15, -22.31750118613795664, -14.56500194951122218 ) ) ;
#7712 = VECTOR ( 'NONE', #1545, 1000.000000000000000 ) ;
#7713 = DIRECTION ( 'NONE',  ( -0.000000000000000000, -1.000000000000000000, -0.000000000000000000 ) ) ;
#7714 = DIRECTION ( 'NONE',  ( 0.000000000000000000, 0.000000000000000000, 1.000000000000000000 ) ) ;
#7715 = ORIENTED_EDGE ( 'NONE', *, *, #18194, .T. ) ;
#7716 = VERTEX_POINT ( 'NONE', #7565 ) ;
#7717 = CARTESIAN_POINT ( 'NONE',  ( 2.769793372871041104, -22.34959508723814992, -1.882086548653340019 ) ) ;
#7718 = CARTESIAN_POINT ( 'NONE',  ( 1.999999999999994449, -28.53928086477465698, -10.43736015284263807 ) ) ;
#7719 = ORIENTED_EDGE ( 'NONE', *, *, #10628, .F. ) ;
#7720 = CARTESIAN_POINT ( 'NONE',  ( 2.500000000000001332, 30.75319992234354416, 0.05647727720530566764 ) ) ;
#7721 = CARTESIAN_POINT ( 'NONE',  ( -2.121784821874996396, -22.19115218676662238, -13.81800486288284624 ) ) ;
#7722 = CARTESIAN_POINT ( 'NONE',  ( 1.135272562821090458, 24.74680007765647716, 3.311245368580554072 ) ) ;
#7723 = CARTESIAN_POINT ( 'NONE',  ( 0.000000000000000000, 20.99999999999999289, 2.500000000000000000 ) ) ;
#7724 = CARTESIAN_POINT ( 'NONE',  ( -0.5553297335970074355, -9.999999999999142020, -4.810349131758192343 ) ) ;
#7725 = STYLED_ITEM ( 'NONE', ( #10690 ), #6498 ) ;
#7726 = CARTESIAN_POINT ( 'NONE',  ( -4.243569643750005227, -27.43435758066657471, -10.62735291601715382 ) ) ;
#7727 = EDGE_CURVE ( 'NONE', #9801, #5271, #17739, .T. ) ;
#7728 = DIRECTION ( 'NONE',  ( 0.000000000000000000, 0.000000000000000000, 1.000000000000000000 ) ) ;
#7729 = EDGE_CURVE ( 'NONE', #5758, #6383, #10348, .T. ) ;
#7730 = CARTESIAN_POINT ( 'NONE',  ( -5.330712181944246111E-15, -28.84980074951425877, -8.377325144622332687 ) ) ;
#7731 = DIRECTION ( 'NONE',  ( 1.000000000000000000, 0.000000000000000000, 0.000000000000000000 ) ) ;
#7732 = ADVANCED_FACE ( 'NONE', ( #11735 ), #15464, .T. ) ;
#7733 = DIRECTION ( 'NONE',  ( 0.000000000000000000, 0.8191520442889952403, -0.5735764363510413855 ) ) ;
#7734 = CARTESIAN_POINT ( 'NONE',  ( 8.500000000000019540, 10.00000000000000000, 20.49999999999998934 ) ) ;
#7735 = CARTESIAN_POINT ( 'NONE',  ( 2.121784821874994176, -26.53427271694390299, -7.206153456172153859 ) ) ;
#7736 = ORIENTED_EDGE ( 'NONE', *, *, #4444, .T. ) ;
#7737 = CARTESIAN_POINT ( 'NONE',  ( -6.158835246850665095E-15, -22.83371997885389248, -15.30223878937131587 ) ) ;
#7738 = DIRECTION ( 'NONE',  ( -0.000000000000000000, 1.000000000000000000, -0.000000000000000000 ) ) ;
#7739 =( GEOMETRIC_REPRESENTATION_CONTEXT ( 3 ) GLOBAL_UNCERTAINTY_ASSIGNED_CONTEXT ( ( #6947 ) ) GLOBAL_UNIT_ASSIGNED_CONTEXT ( ( #10172, #12958, #557 ) ) REPRESENTATION_CONTEXT ( 'NONE', 'WORKASPACE' ) );
#7740 = ADVANCED_FACE ( 'NONE', ( #9240 ), #1941, .T. ) ;
#7741 = CARTESIAN_POINT ( 'NONE',  ( -2.055738996568313048, 30.74680007765648071, -1.423772053676023441 ) ) ;
#7742 = EDGE_LOOP ( 'NONE', ( #10361, #12844, #15825, #17158 ) ) ;
#7743 = CARTESIAN_POINT ( 'NONE',  ( -2.864755990943265829, 28.24680007765648071, -2.011557305968488141 ) ) ;
#7744 = CARTESIAN_POINT ( 'NONE',  ( 1.743066579297358403E-15, -23.41446612136426708, -16.13163023522068684 ) ) ;
#7745 = SHAPE_DEFINITION_REPRESENTATION ( #725, #12769 ) ;
#7746 = LINE ( 'NONE', #8954, #10141 ) ;
#7747 = EDGE_LOOP ( 'NONE', ( #8987, #2085, #4461, #1854 ) ) ;
#7748 = CIRCLE ( 'NONE', #17250, 0.1999999999999987899 ) ;
#7749 = CARTESIAN_POINT ( 'NONE',  ( -4.243569643750000786, -22.35161007189942595, -7.639927304239214401 ) ) ;
#7750 = CARTESIAN_POINT ( 'NONE',  ( -3.607379964056306676, 37.74680007765647360, 2.690724712371306282 ) ) ;
#7751 = ORIENTED_EDGE ( 'NONE', *, *, #13676, .F. ) ;
#7752 = COLOUR_RGB ( '',1.000000000000000000, 0.9490196078431372140, 0.9098039215686274384 ) ;
#7753 =( NAMED_UNIT ( * ) PLANE_ANGLE_UNIT ( ) SI_UNIT ( $, .RADIAN. ) );
#7754 = LINE ( 'NONE', #12107, #12993 ) ;
#7755 = CARTESIAN_POINT ( 'NONE',  ( -4.025001148619858249, -27.33870370935842686, -14.18005106542060467 ) ) ;
#7756 = CARTESIAN_POINT ( 'NONE',  ( -4.648177544792955347E-16, -30.03220982406077155, -11.63517334838810058 ) ) ;
#7757 = CARTESIAN_POINT ( 'NONE',  ( 7.496325586166000754, -13.00735673026645856, 5.000734971399987572 ) ) ;
#7758 = CARTESIAN_POINT ( 'NONE',  ( 2.000000000000004441, -20.77764473892288777, -11.43154871188538557 ) ) ;
#7759 = CARTESIAN_POINT ( 'NONE',  ( 4.243569643749996345, -22.70235198077049787, -3.869348550632942363 ) ) ;
#7760 = ORIENTED_EDGE ( 'NONE', *, *, #4955, .T. ) ;
#7761 = DIRECTION ( 'NONE',  ( -1.000000000000000000, -0.000000000000000000, -0.000000000000000000 ) ) ;
#7762 = AXIS2_PLACEMENT_3D ( 'NONE', #8574, #7093, #345 ) ;
#7763 = CARTESIAN_POINT ( 'NONE',  ( -4.000000000000000888, -23.78734358949309424, -9.690367265603486047 ) ) ;
#7764 = PRESENTATION_LAYER_ASSIGNMENT (  '', '', ( #1851 ) ) ;
#7765 = ORIENTED_EDGE ( 'NONE', *, *, #1981, .T. ) ;
#7766 = EDGE_LOOP ( 'NONE', ( #16332, #4622, #13343, #5602 ) ) ;
#7767 = DIRECTION ( 'NONE',  ( -1.000000000000000000, 0.000000000000000000, 4.336808689942021680E-16 ) ) ;
#7768 = FILL_AREA_STYLE ('',( #10547 ) ) ;
#7769 = CARTESIAN_POINT ( 'NONE',  ( 0.05938372350919016857, 22.62819992234354416, -4.731580009072201776 ) ) ;
#7770 = CARTESIAN_POINT ( 'NONE',  ( -3.500000000000000444, 39.50319992234354061, -0.05647727720529600870 ) ) ;
#7771 = CARTESIAN_POINT ( 'NONE',  ( -2.500000000000001332, 19.50319992234354771, -0.05647727720530596601 ) ) ;
#7772 = VERTEX_POINT ( 'NONE', #6275 ) ;
#7773 = CARTESIAN_POINT ( 'NONE',  ( -4.518350579753632523, 15.62180007765647360, -1.405661355842698468 ) ) ;
#7774 = CARTESIAN_POINT ( 'NONE',  ( 1.999999999999994449, -24.40953052304715953, -4.539465433961872520 ) ) ;
#7775 = EDGE_LOOP ( 'NONE', ( #13991, #4317, #15928, #5267 ) ) ;
#7776 = AXIS2_PLACEMENT_3D ( 'NONE', #3543, #12143, #764 ) ;
#7777 = CARTESIAN_POINT ( 'NONE',  ( 4.000000000000000000, -1.759474945355388176, -3.047499999999998099 ) ) ;
#7778 = AXIS2_PLACEMENT_3D ( 'NONE', #265, #3329, #15941 ) ;
#7779 = CARTESIAN_POINT ( 'NONE',  ( 0.000000000000000000, 3.518949890710770134, -4.119968255444916849E-15 ) ) ;
#7780 = ADVANCED_FACE ( 'NONE', ( #2031 ), #4882, .T. ) ;
#7781 = DIRECTION ( 'NONE',  ( 0.000000000000000000, 0.000000000000000000, 1.000000000000000000 ) ) ;
#7782 = CARTESIAN_POINT ( 'NONE',  ( 3.999999999999996447, -26.60398620621909416, -9.686631897307085737 ) ) ;
#7783 = CARTESIAN_POINT ( 'NONE',  ( -5.330712181944246111E-15, -24.46194101142878807, -2.110812005811521619 ) ) ;
#7784 = CARTESIAN_POINT ( 'NONE',  ( -4.243569643749997233, -22.68915988664961247, -12.39348851099227389 ) ) ;
#7785 = EDGE_CURVE ( 'NONE', #297, #13721, #8959, .T. ) ;
#7786 = VERTEX_POINT ( 'NONE', #4793 ) ;
#7787 = CARTESIAN_POINT ( 'NONE',  ( 4.299564228933482956E-15, -16.63909446626264454, -6.455396711050170211 ) ) ;
#7788 = CARTESIAN_POINT ( 'NONE',  ( 4.898587196589413815E-16, 2.700915433685006750, 35.11257424290206330 ) ) ;
#7789 = AXIS2_PLACEMENT_3D ( 'NONE', #13127, #16019, #9048 ) ;
#7790 = DIRECTION ( 'NONE',  ( 0.000000000000000000, 0.8191520442889952403, -0.5735764363510413855 ) ) ;
#7791 = CARTESIAN_POINT ( 'NONE',  ( -4.243569643750000786, -26.48136041362692339, -13.53782202311997551 ) ) ;
#7792 = VERTEX_POINT ( 'NONE', #3228 ) ;
#7793 = AXIS2_PLACEMENT_3D ( 'NONE', #16063, #3539, #6028 ) ;
#7794 = CARTESIAN_POINT ( 'NONE',  ( -2.798362969681409851, 24.75319992234354416, -2.102939460078765421 ) ) ;
#7795 = DIRECTION ( 'NONE',  ( -0.9454169814551723894, 0.000000000000000000, 0.3258630558627204632 ) ) ;
#7796 = CARTESIAN_POINT ( 'NONE',  ( 4.243569643749996345, -23.70252589165761492, -5.297744927861876896 ) ) ;
#7797 = CARTESIAN_POINT ( 'NONE',  ( -2.481649420246374138, 22.87180007765648071, 0.8687765177876256573 ) ) ;
#7798 = CARTESIAN_POINT ( 'NONE',  ( -3.673772985318163098, 19.25319992234354416, 2.599342558261029001 ) ) ;
#7799 = CARTESIAN_POINT ( 'NONE',  ( 4.243569643750003451, -24.06574333389211873, -14.35945341728585767 ) ) ;
#7800 = CARTESIAN_POINT ( 'NONE',  ( 4.000000000000000888, -26.69107429781530527, -13.83732448880975419 ) ) ;
#7801 = CARTESIAN_POINT ( 'NONE',  ( -2.121784821874996396, -17.83555612322590278, -7.597569026563290251 ) ) ;
#7802 = CARTESIAN_POINT ( 'NONE',  ( -3.518350579753630747, 15.62180007765647538, -1.080741659609802729 ) ) ;
#7803 = TOROIDAL_SURFACE ( 'NONE', #3966, 9.000000000000001776, 0.9999999999999991118 ) ;
#7804 = ADVANCED_FACE ( 'NONE', ( #17530, #7378 ), #353, .T. ) ;
#7805 = CARTESIAN_POINT ( 'NONE',  ( -8.500000000000005329, 13.00000000000000178, -18.35000000000000142 ) ) ;
#7806 = CARTESIAN_POINT ( 'NONE',  ( 4.000000000000000888, -20.23833938886609118, -4.621863990558560786 ) ) ;
#7807 = CYLINDRICAL_SURFACE ( 'NONE', #15363, 4.000000000000000000 ) ;
#7808 = ORIENTED_EDGE ( 'NONE', *, *, #12676, .F. ) ;
#7809 = ORIENTED_EDGE ( 'NONE', *, *, #14860, .F. ) ;
#7810 = CARTESIAN_POINT ( 'NONE',  ( -1.999999999999996225, -16.86298556082702760, -5.840836009612994317 ) ) ;
#7811 = CARTESIAN_POINT ( 'NONE',  ( 2.000000000000004441, -22.77799255999219952, -14.28834146533649196 ) ) ;
#7812 = ORIENTED_EDGE ( 'NONE', *, *, #12676, .T. ) ;
#7813 = CARTESIAN_POINT ( 'NONE',  ( -1.497042530366522461, 32.37819992234353350, -2.161531897785030409 ) ) ;
#7814 = FILL_AREA_STYLE ('',( #3288 ) ) ;
#7815 = CARTESIAN_POINT ( 'NONE',  ( -4.243569643749997233, -23.17311500482080433, -13.08464804836111206 ) ) ;
#7816 = CARTESIAN_POINT ( 'NONE',  ( -3.518350579753630747, 25.62180007765648071, -1.080741659609802729 ) ) ;
#7817 = CARTESIAN_POINT ( 'NONE',  ( -1.734723475976807094E-15, 38.59999999999999432, -2.500000000000000000 ) ) ;
#7818 = FACE_OUTER_BOUND ( 'NONE', #9145, .T. ) ;
#7819 = CIRCLE ( 'NONE', #9592, 8.000000000000000000 ) ;
#7820 = CARTESIAN_POINT ( 'NONE',  ( -2.121784821875005722, -28.93253919143669251, -10.63123294135551689 ) ) ;
#7821 = DIRECTION ( 'NONE',  ( -1.000000000000000000, 0.000000000000000000, 0.000000000000000000 ) ) ;
#7822 = MANIFOLD_SOLID_BREP ( 'LPattern6[1]', #11169 ) ;
#7823 = DIRECTION ( 'NONE',  ( -6.162975822039154730E-33, 0.5735764363510414965, 0.8191520442889950182 ) ) ;
#7824 = DIRECTION ( 'NONE',  ( 0.000000000000000000, -0.4999999999999992784, 0.8660254037844389297 ) ) ;
#7825 = CARTESIAN_POINT ( 'NONE',  ( -2.121784821874996396, -20.38438641226084158, -11.23767592337251209 ) ) ;
#7826 = ORIENTED_EDGE ( 'NONE', *, *, #813, .T. ) ;
#7827 = DIRECTION ( 'NONE',  ( -0.000000000000000000, -0.5735764363510414965, -0.8191520442889950182 ) ) ;
#7828 = DIRECTION ( 'NONE',  ( -3.469446951953613696E-16, -0.000000000000000000, -1.000000000000000000 ) ) ;
#7829 = CARTESIAN_POINT ( 'NONE',  ( 0.05938372350926800214, 32.37180007765648782, 2.628655560595669183 ) ) ;
#7830 = ORIENTED_EDGE ( 'NONE', *, *, #12879, .F. ) ;
#7831 = CARTESIAN_POINT ( 'NONE',  ( 3.481649420246370141, 31.62180007765647005, -1.193696214020541602 ) ) ;
#7832 = DIRECTION ( 'NONE',  ( 1.049727191973305394E-16, 0.5150380737757255245, -0.8571673013836856869 ) ) ;
#7833 = ADVANCED_FACE ( 'NONE', ( #15003 ), #3412, .F. ) ;
#7834 = CARTESIAN_POINT ( 'NONE',  ( -8.000000000000000000, 46.00000000000000000, 2.499999999999999112 ) ) ;
#7835 = EDGE_CURVE ( 'NONE', #8639, #985, #10110, .T. ) ;
#7836 = ADVANCED_BREP_SHAPE_REPRESENTATION ( '', ( #2218, #16940 ), #7446 ) ;
#7837 = APPLICATION_CONTEXT ( 'automotive_design' ) ;
#7838 = ORIENTED_EDGE ( 'NONE', *, *, #1381, .T. ) ;
#7839 = CARTESIAN_POINT ( 'NONE',  ( 4.730628863548789710E-15, -18.14414028696156578, -10.17401794073526311 ) ) ;
#7840 = ADVANCED_FACE ( 'NONE', ( #16671 ), #4264, .T. ) ;
#7841 = CARTESIAN_POINT ( 'NONE',  ( 2.733110507866247652, 38.87180007765646650, -3.862833514489153686 ) ) ;
#7842 = VERTEX_POINT ( 'NONE', #2300 ) ;
#7843 = EDGE_CURVE ( 'NONE', #3136, #7134, #10786, .T. ) ;
#7844 = CARTESIAN_POINT ( 'NONE',  ( 9.000000000000005329, 27.59999999999999432, 2.499999999999997335 ) ) ;
#7845 = CARTESIAN_POINT ( 'NONE',  ( -9.000000000000001776, 20.99999999999999289, 2.499999999999995559 ) ) ;
#7846 = CARTESIAN_POINT ( 'NONE',  ( -3.577231619497362125, -28.57177006857940782, -13.28786742256294495 ) ) ;
#7847 = CARTESIAN_POINT ( 'NONE',  ( 7.252352847715823891, -10.36846725531173163, 4.245760260470595071 ) ) ;
#7848 = CARTESIAN_POINT ( 'NONE',  ( -1.999999999999996225, -18.92786073169077454, -8.789783369053376205 ) ) ;
#7849 = CARTESIAN_POINT ( 'NONE',  ( 4.730628863548789710E-15, -16.59548390881375468, -7.962307421154977582 ) ) ;
#7850 = EDGE_LOOP ( 'NONE', ( #10725, #8342, #8661, #7681 ) ) ;
#7851 = DIRECTION ( 'NONE',  ( -3.373073425510457965E-16, 0.000000000000000000, -1.000000000000000000 ) ) ;
#7852 = CARTESIAN_POINT ( 'NONE',  ( -2.000000000000005773, -25.54951369099979175, -6.167530122993019503 ) ) ;
#7853 = VERTEX_POINT ( 'NONE', #999 ) ;
#7854 = EDGE_LOOP ( 'NONE', ( #15580, #11538, #8532, #1093 ) ) ;
#7855 = DIRECTION ( 'NONE',  ( 0.000000000000000000, 0.000000000000000000, 1.000000000000000000 ) ) ;
#7856 = CARTESIAN_POINT ( 'NONE',  ( -4.499999999999999112, 34.50319992234354771, -0.05647727720528529505 ) ) ;
#7857 = CARTESIAN_POINT ( 'NONE',  ( 0.05938372350920110426, 37.62819992234353350, -3.680117784833935701 ) ) ;
#7858 = CARTESIAN_POINT ( 'NONE',  ( -1.593127413382952939, 24.12819992234354771, 2.091722143975172532 ) ) ;
#7859 = AXIS2_PLACEMENT_3D ( 'NONE', #2819, #12723, #5768 ) ;
#7860 = EDGE_LOOP ( 'NONE', ( #5305, #8129, #11187, #10956 ) ) ;
#7861 = CARTESIAN_POINT ( 'NONE',  ( -3.673772985318219053, 20.74680007765647716, -2.599342558260952174 ) ) ;
#7862 = CARTESIAN_POINT ( 'NONE',  ( 4.713407268011036227E-15, -17.16463900263063636, -8.284800724790995829 ) ) ;
#7863 = ORIENTED_EDGE ( 'NONE', *, *, #12940, .F. ) ;
#7864 = LINE ( 'NONE', #10470, #4108 ) ;
#7865 = CARTESIAN_POINT ( 'NONE',  ( -3.500000000000000444, 35.49680007765648071, 0.05647727720536892260 ) ) ;
#7866 = CARTESIAN_POINT ( 'NONE',  ( 8.500000000000019540, 10.00000000000000000, 22.49999999999999289 ) ) ;
#7867 = DIRECTION ( 'NONE',  ( 0.000000000000000000, 0.5000000000000001110, -0.8660254037844385966 ) ) ;
#7868 = AXIS2_PLACEMENT_3D ( 'NONE', #10875, #8367, #17950 ) ;
#7869 = CARTESIAN_POINT ( 'NONE',  ( -5.330712181944245322E-15, -28.10773623498509721, -7.317547187323446778 ) ) ;
#7870 = CARTESIAN_POINT ( 'NONE',  ( 4.000000000000003553, -24.58423252177867369, -14.85476051292054578 ) ) ;
#7871 = VERTEX_POINT ( 'NONE', #6546 ) ;
#7872 = CIRCLE ( 'NONE', #17070, 2.149999999999995470 ) ;
#7873 = CARTESIAN_POINT ( 'NONE',  ( -4.386042834387951395, -10.00000000000000178, 22.42214358049744760 ) ) ;
#7874 =( NAMED_UNIT ( * ) SI_UNIT ( $, .STERADIAN. ) SOLID_ANGLE_UNIT ( ) );
#7875 = DIRECTION ( 'NONE',  ( 0.000000000000000000, 0.000000000000000000, 1.000000000000000000 ) ) ;
#7876 = CARTESIAN_POINT ( 'NONE',  ( 4.243569643750003451, -24.84007152296602428, -15.46530867707600088 ) ) ;
#7877 = ORIENTED_EDGE ( 'NONE', *, *, #6882, .F. ) ;
#7878 = CARTESIAN_POINT ( 'NONE',  ( 3.500000000000000444, 33.25319992234354771, 0.05647727720529520379 ) ) ;
#7879 = DIRECTION ( 'NONE',  ( -1.000000000000000000, -0.000000000000000000, -0.000000000000000000 ) ) ;
#7880 = CARTESIAN_POINT ( 'NONE',  ( -2.121784821875005722, -23.73808758973257227, -3.212787240263307531 ) ) ;
#7881 = CARTESIAN_POINT ( 'NONE',  ( 2.055738996568313048, 21.99680007765648426, 1.423772053676023441 ) ) ;
#7882 = CARTESIAN_POINT ( 'NONE',  ( 0.05938372350919016857, 15.12819992234354594, -4.731580009072201776 ) ) ;
#7883 = CARTESIAN_POINT ( 'NONE',  ( 4.000000000000000888, -25.65863671238343358, -12.36285080908956502 ) ) ;
#7884 = ORIENTED_EDGE ( 'NONE', *, *, #8063, .F. ) ;
#7885 = CARTESIAN_POINT ( 'NONE',  ( 4.243569643750000786, -20.67389899557263533, -5.243907574693898788 ) ) ;
#7886 = VECTOR ( 'NONE', #12108, 1000.000000000000000 ) ;
#7887 = CARTESIAN_POINT ( 'NONE',  ( 4.499999999999999112, 39.24680007765647360, -0.05647727720537982360 ) ) ;
#7888 = B_SPLINE_CURVE_WITH_KNOTS ( 'NONE', 3,
 ( #13778, #17710, #7846, #15006, #6728, #4974, #7755, #18072, #16673, #2125, #10630, #2302, #16304, #3590, #9242, #3683, #13499, #814, #6458, #5065, #10721, #10813, #9329, #3860, #16396, #17980, #6549, #16488, #3766, #2396, #13685, #6642, #1001, #15186 ),
 .UNSPECIFIED., .F., .F.,
 ( 4, 2, 2, 2, 2, 2, 2, 2, 2, 2, 2, 2, 2, 2, 2, 2, 4 ),
 ( 0.007412722934092349537, 0.008215427948509459316, 0.009018132962926569962, 0.009820837977343680608, 0.01062354299176079125, 0.01142624800617790190, 0.01222895302059501255, 0.01303165803501212319, 0.01383436304942923384, 0.01463706806384634448, 0.01543977307826345513, 0.01624247809268056578, 0.01704518310709767295, 0.01784788812151478360, 0.01865059313593189425, 0.01945329815034900489, 0.02025600316476611554 ),
 .UNSPECIFIED. ) ;
#7889 = DIRECTION ( 'NONE',  ( 0.000000000000000000, 0.000000000000000000, 1.000000000000000000 ) ) ;
#7890 = CARTESIAN_POINT ( 'NONE',  ( 1.300000000000000044, 0.000000000000000000, 0.000000000000000000 ) ) ;
#7891 = DIRECTION ( 'NONE',  ( -0.7071067811865484609, 0.000000000000000000, 0.7071067811865465735 ) ) ;
#7892 = ORIENTED_EDGE ( 'NONE', *, *, #10176, .T. ) ;
#7893 = ORIENTED_EDGE ( 'NONE', *, *, #1626, .F. ) ;
#7894 =( BOUNDED_CURVE ( )  B_SPLINE_CURVE ( 2, ( #1849, #15588, #3236, #4803, #547, #11840, #9915, #6192, #17440 ),
 .UNSPECIFIED., .F., .T. ) 
 B_SPLINE_CURVE_WITH_KNOTS ( ( 3, 2, 2, 2, 3 ),
 ( 0.4568965517241379559, 0.4597701149425287293, 0.4655172413793103314, 0.4712643678160919336, 0.4741379310344827624 ),
 .UNSPECIFIED. ) 
 CURVE ( )  GEOMETRIC_REPRESENTATION_ITEM ( )  RATIONAL_B_SPLINE_CURVE ( ( 0.9330127018922194093, 0.9330127018922200755, 1.000000000000000000, 0.8660254037844387076, 1.000000000000000000, 0.8660254037844387076, 1.000000000000000000, 0.9330127018922187432, 0.9330127018922194093 ) ) 
 REPRESENTATION_ITEM ( '' )  );
#7895 = CARTESIAN_POINT ( 'NONE',  ( 2.115076519116362963, 16.37180007765647716, -3.012182706137107147 ) ) ;
#7896 = EDGE_CURVE ( 'NONE', #15565, #13882, #2216, .T. ) ;
#7897 = CARTESIAN_POINT ( 'NONE',  ( 4.000000000000003553, -24.84234191813664339, -15.22337893285059707 ) ) ;
#7898 = CARTESIAN_POINT ( 'NONE',  ( 2.000000000000004441, -21.22933618184438842, -12.07663094575620377 ) ) ;
#7899 = VERTEX_POINT ( 'NONE', #10992 ) ;
#7900 = CARTESIAN_POINT ( 'NONE',  ( -2.055738996568281518, 26.75319992234354771, 1.423772053676066962 ) ) ;
#7901 = SURFACE_STYLE_USAGE ( .BOTH. , #874 ) ;
#7902 = CIRCLE ( 'NONE', #10856, 2.149999999999995470 ) ;
#7903 = CARTESIAN_POINT ( 'NONE',  ( -4.243569643749997233, -22.39878681574689523, -11.97879278857096885 ) ) ;
#7904 = CARTESIAN_POINT ( 'NONE',  ( 3.481649420246369697, 24.12180007765648071, -1.193696214020541824 ) ) ;
#7905 = DIRECTION ( 'NONE',  ( 0.000000000000000000, 0.8191520442889952403, -0.5735764363510413855 ) ) ;
#7906 = EDGE_CURVE ( 'NONE', #4967, #6724, #11404, .T. ) ;
#7907 = CARTESIAN_POINT ( 'NONE',  ( -1.661723472263481630E-14, -20.76884480799014554, -12.35329142993093576 ) ) ;
#7908 = CARTESIAN_POINT ( 'NONE',  ( -2.121784821874996396, -22.22341586131136992, -13.86408216537410354 ) ) ;
#7909 = AXIS2_PLACEMENT_3D ( 'NONE', #6630, #2041, #8013 ) ;
#7910 = AXIS2_PLACEMENT_3D ( 'NONE', #8496, #12433, #17151 ) ;
#7911 = CARTESIAN_POINT ( 'NONE',  ( 3.497645065122034769, -25.34683430723604403, -15.74138193774221328 ) ) ;
#7912 = CARTESIAN_POINT ( 'NONE',  ( 3.607379964056306676, 21.49680007765647360, -2.690724712371305838 ) ) ;
#7913 = LINE ( 'NONE', #11813, #9176 ) ;
#7914 = CARTESIAN_POINT ( 'NONE',  ( 1.820000000000000062, 0.000000000000000000, 3.799999999999999378 ) ) ;
#7915 = CARTESIAN_POINT ( 'NONE',  ( -2.121784821874996396, -19.86816761954490573, -10.50043908351241662 ) ) ;
#7916 = ORIENTED_EDGE ( 'NONE', *, *, #4453, .F. ) ;
#7917 = LINE ( 'NONE', #2109, #11871 ) ;
#7918 = LINE ( 'NONE', #10704, #15396 ) ;
#7919 = CARTESIAN_POINT ( 'NONE',  ( -2.481649420246374138, 30.37180007765648426, 0.8687765177876256573 ) ) ;
#7920 = ORIENTED_EDGE ( 'NONE', *, *, #12163, .T. ) ;
#7921 = CARTESIAN_POINT ( 'NONE',  ( 0.05938372350927906967, 29.87180007765647716, 3.680117784833935701 ) ) ;
#7922 = CLOSED_SHELL ( 'NONE', ( #17569, #2488, #10265, #16458, #945, #3506, #16836, #8167, #12633, #10624 ) ) ;
#7923 = CARTESIAN_POINT ( 'NONE',  ( -4.000000000000004441, -21.97952618743386566, -3.082218539220304976 ) ) ;
#7924 = DIRECTION ( 'NONE',  ( -6.162975822039154730E-33, 0.5735764363510414965, 0.8191520442889950182 ) ) ;
#7925 = VECTOR ( 'NONE', #3051, 1000.000000000000000 ) ;
#7926 = CARTESIAN_POINT ( 'NONE',  ( 0.000000000000000000, 0.000000000000000000, 0.000000000000000000 ) ) ;
#7927 = AXIS2_PLACEMENT_3D ( 'NONE', #14122, #16841, #14034 ) ;
#7928 = ORIENTED_EDGE ( 'NONE', *, *, #16926, .T. ) ;
#7929 = CARTESIAN_POINT ( 'NONE',  ( 4.243569643750003451, -21.22653997395446623, -10.30465079805533080 ) ) ;
#7930 = CARTESIAN_POINT ( 'NONE',  ( 3.500000000000000444, 24.24680007765647716, -0.05647727720536935281 ) ) ;
#7931 = ORIENTED_EDGE ( 'NONE', *, *, #11015, .F. ) ;
#7932 = DIRECTION ( 'NONE',  ( -0.000000000000000000, 1.000000000000000000, -0.000000000000000000 ) ) ;
#7933 = EDGE_CURVE ( 'NONE', #4719, #3449, #6080, .T. ) ;
#7934 = CARTESIAN_POINT ( 'NONE',  ( 0.000000000000000000, 16.59999999999999787, 2.500000000000000000 ) ) ;
#7935 = CIRCLE ( 'NONE', #4374, 0.4000000000000006883 ) ;
#7936 = CARTESIAN_POINT ( 'NONE',  ( 6.772399938786841211, -14.05066417492660591, -1.433852700220792142 ) ) ;
#7938 = DIRECTION ( 'NONE',  ( 0.000000000000000000, 0.4999999999999990008, -0.8660254037844391517 ) ) ;
#7937 = AXIS2_PLACEMENT_3D ( 'NONE', #2358, #13643, #960 ) ;
#7939 = CARTESIAN_POINT ( 'NONE',  ( -4.243569643749997233, -24.97988077932658513, -15.66497698787144977 ) ) ;
#7940 = EDGE_CURVE ( 'NONE', #13373, #3130, #10902, .T. ) ;
#7941 = ORIENTED_EDGE ( 'NONE', *, *, #11537, .T. ) ;
#7942 = CARTESIAN_POINT ( 'NONE',  ( -5.577813053751546416E-15, -28.54808079570739920, -9.515617434797091434 ) ) ;
#7943 = CARTESIAN_POINT ( 'NONE',  ( -1.999999999999996225, -20.73462650619655534, -11.37011230856371036 ) ) ;
#7944 = CARTESIAN_POINT ( 'NONE',  ( -2.864755990943265829, 33.24680007765648071, -2.011557305968488141 ) ) ;
#7945 = ORIENTED_EDGE ( 'NONE', *, *, #548, .F. ) ;
#7946 = ORIENTED_EDGE ( 'NONE', *, *, #592, .F. ) ;
#7947 = APPLICATION_CONTEXT ( 'automotive_design' ) ;
#7948 =( LENGTH_UNIT ( ) NAMED_UNIT ( * ) SI_UNIT ( .MILLI., .METRE. ) );
#7949 = CARTESIAN_POINT ( 'NONE',  ( 4.499999999999999112, 30.75319992234354416, 0.05647727720528474687 ) ) ;
#7950 = CARTESIAN_POINT ( 'NONE',  ( 2.115076519116425580, 36.12819992234355482, 3.012182706137062294 ) ) ;
#7951 = CARTESIAN_POINT ( 'NONE',  ( -2.481649420246391902, 29.62819992234354416, -0.8687765177875723666 ) ) ;
#7952 = EDGE_LOOP ( 'NONE', ( #14881, #6957, #3541, #11741 ) ) ;
#7953 = CARTESIAN_POINT ( 'NONE',  ( 3.673772985318219053, 24.49680007765648071, 2.599342558260951730 ) ) ;
#7954 = AXIS2_PLACEMENT_3D ( 'NONE', #5927, #11479, #17172 ) ;
#7955 = CARTESIAN_POINT ( 'NONE',  ( -3.999999999999997335, -18.75526198665626154, -6.530127861826874103 ) ) ;
#7956 = EDGE_LOOP ( 'NONE', ( #14367, #4071, #8081, #2597 ) ) ;
#7957 = DIRECTION ( 'NONE',  ( 0.000000000000000000, 0.000000000000000000, -1.000000000000000000 ) ) ;
#7958 = DIRECTION ( 'NONE',  ( 0.000000000000000000, 0.000000000000000000, 1.000000000000000000 ) ) ;
#7959 = EDGE_CURVE ( 'NONE', #14652, #17766, #17885, .T. ) ;
#7960 = DIRECTION ( 'NONE',  ( 0.000000000000000000, -1.000000000000000000, 0.000000000000000000 ) ) ;
#7961 = EDGE_CURVE ( 'NONE', #18219, #2970, #10606, .T. ) ;
#7962 = DIRECTION ( 'NONE',  ( 0.000000000000000000, -0.8660254037844385966, -0.5000000000000001110 ) ) ;
#7963 = EDGE_CURVE ( 'NONE', #5212, #12374, #8759, .T. ) ;
#7964 = CARTESIAN_POINT ( 'NONE',  ( 2.121784821874994176, -27.08275518420459349, -7.989467598523504854 ) ) ;
#7965 = PRODUCT_DEFINITION_SHAPE ( 'NONE', 'NONE',  #18370 ) ;
#7966 = CIRCLE ( 'NONE', #10327, 10.00000000000000178 ) ;
#7967 = CARTESIAN_POINT ( 'NONE',  ( -1.071796769724505882, -19.72488052183944163, -10.86235591555482038 ) ) ;
#7968 = VECTOR ( 'NONE', #14853, 1000.000000000000000 ) ;
#7969 = EDGE_LOOP ( 'NONE', ( #9908, #15671 ) ) ;
#7970 = PRODUCT_DEFINITION_CONTEXT ( 'detailed design', #3111, 'design' ) ;
#7971 = CARTESIAN_POINT ( 'NONE',  ( -5.694236848974727927, -11.38679575279407530, 16.60313092159233861 ) ) ;
#7972 = DIRECTION ( 'NONE',  ( -0.000000000000000000, 1.000000000000000000, -0.000000000000000000 ) ) ;
#7973 = CARTESIAN_POINT ( 'NONE',  ( -4.000000000000000888, -22.69037865426678380, -8.123738979894017831 ) ) ;
#7974 = CARTESIAN_POINT ( 'NONE',  ( 4.730628863548789710E-15, -22.27389062868906677, -16.07191265961602511 ) ) ;
#7975 = VERTEX_POINT ( 'NONE', #17801 ) ;
#7976 = CARTESIAN_POINT ( 'NONE',  ( -2.864755990943222308, 39.25319992234354771, 2.011557305968548093 ) ) ;
#7977 = CARTESIAN_POINT ( 'NONE',  ( -10.00000000000000000, 16.59999999999999787, 2.499999999999998224 ) ) ;
#7978 = CARTESIAN_POINT ( 'NONE',  ( 4.243569643750003451, -18.35507293947206264, -6.203770876333551954 ) ) ;
#7979 = CARTESIAN_POINT ( 'NONE',  ( -2.518350579753628526, 30.62180007765647716, -0.7558219633769075463 ) ) ;
#7980 = CARTESIAN_POINT ( 'NONE',  ( -2.733110507866328476, 19.87819992234354416, -3.862833514489096398 ) ) ;
#7981 = CARTESIAN_POINT ( 'NONE',  ( -1.999999999999996225, -21.70253674183399184, -12.75243138229462758 ) ) ;
#7982 = ORIENTED_EDGE ( 'NONE', *, *, #5352, .T. ) ;
#7983 = CARTESIAN_POINT ( 'NONE',  ( -5.577813053751546416E-15, -28.80619019206536535, -9.884235854727139170 ) ) ;
#7984 = CARTESIAN_POINT ( 'NONE',  ( -3.500000000000000444, 17.99680007765647716, 0.05647727720536892260 ) ) ;
#7985 = CARTESIAN_POINT ( 'NONE',  ( -4.000000000000007105, 0.000000000000000000, 30.00000000000000000 ) ) ;
#7986 = CARTESIAN_POINT ( 'NONE',  ( 1.071796769724485232, -24.66491314961903569, -3.969879301190459842 ) ) ;
#7987 = CARTESIAN_POINT ( 'NONE',  ( 3.999999999999993339, 7.428752623566170548E-15, 30.00000000000000000 ) ) ;
#7988 = ORIENTED_EDGE ( 'NONE', *, *, #11691, .F. ) ;
#7989 = ORIENTED_EDGE ( 'NONE', *, *, #5422, .T. ) ;
#7990 = CARTESIAN_POINT ( 'NONE',  ( 8.500000000000001776, 14.80000000000000071, -20.49999999999999645 ) ) ;
#7992 = ADVANCED_FACE ( 'NONE', ( #5063 ), #2574, .F. ) ;
#7991 = DIRECTION ( 'NONE',  ( 1.000000000000000000, 0.000000000000000000, 0.000000000000000000 ) ) ;
#7993 = CARTESIAN_POINT ( 'NONE',  ( 2.000000000000004441, -23.03610195635016922, -14.65695988526653792 ) ) ;
#7994 = ORIENTED_EDGE ( 'NONE', *, *, #18330, .T. ) ;
#7995 = AXIS2_PLACEMENT_3D ( 'NONE', #15630, #1820, #11531 ) ;
#7996 = CARTESIAN_POINT ( 'NONE',  ( -2.115076519116425580, 14.87819992234354594, -3.012182706137062738 ) ) ;
#7997 = CARTESIAN_POINT ( 'NONE',  ( -4.243569643750000786, -23.86800277550248950, -9.805560521328242629 ) ) ;
#7998 = CARTESIAN_POINT ( 'NONE',  ( -0.05938372350927861171, 31.12180007765647005, -3.680117784833935701 ) ) ;
#7999 = CARTESIAN_POINT ( 'NONE',  ( 2.798362969681409851, 16.00319992234354416, 2.102939460078764977 ) ) ;
#8000 = CARTESIAN_POINT ( 'NONE',  ( -8.500000000000007105, 14.80000000000000071, -20.49999999999999645 ) ) ;
#8001 = CYLINDRICAL_SURFACE ( 'NONE', #6098, 4.000000000000000000 ) ;
#8002 = CARTESIAN_POINT ( 'NONE',  ( 4.243569643750003451, -23.03330574846024703, -12.88497973756566672 ) ) ;
#8003 =( BOUNDED_CURVE ( )  B_SPLINE_CURVE ( 2, ( #6164, #519, #6352, #17510, #886, #705, #15072, #5044, #10793 ),
 .UNSPECIFIED., .F., .F. ) 
 B_SPLINE_CURVE_WITH_KNOTS ( ( 3, 2, 2, 2, 3 ),
 ( 0.9051724137931034253, 0.9080459770114942541, 0.9137931034482759118, 0.9195402298850574585, 0.9224137931034482873 ),
 .UNSPECIFIED. ) 
 CURVE ( )  GEOMETRIC_REPRESENTATION_ITEM ( )  RATIONAL_B_SPLINE_CURVE ( ( 0.9330127018922194093, 0.9330127018922194093, 1.000000000000000000, 0.8660254037844387076, 1.000000000000000000, 0.8660254037844387076, 1.000000000000000000, 0.9330127018922194093, 0.9330127018922194093 ) ) 
 REPRESENTATION_ITEM ( '' )  );
#8004 = DIRECTION ( 'NONE',  ( -0.000000000000000000, -1.000000000000000000, -0.000000000000000000 ) ) ;
#8005 = ADVANCED_FACE ( 'NONE', ( #15183 ), #8207, .F. ) ;
#8006 = CARTESIAN_POINT ( 'NONE',  ( 3.673772985318219053, 26.99680007765647716, 2.599342558260951730 ) ) ;
#8007 = CARTESIAN_POINT ( 'NONE',  ( 9.000000000000000000, 23.19999999999999574, -2.500000000000001332 ) ) ;
#8008 = DIRECTION ( 'NONE',  ( 0.000000000000000000, 0.000000000000000000, 1.000000000000000000 ) ) ;
#8009 = CARTESIAN_POINT ( 'NONE',  ( 4.243569643750000786, -21.41596351010179333, -6.303685531992786473 ) ) ;
#8010 = ORIENTED_EDGE ( 'NONE', *, *, #13846, .T. ) ;
#8011 = EDGE_CURVE ( 'NONE', #3470, #9679, #13272, .T. ) ;
#8012 = CARTESIAN_POINT ( 'NONE',  ( -1.999999999999996225, -19.18597012804874069, -9.158401788983423941 ) ) ;
#8013 = DIRECTION ( 'NONE',  ( 1.000000000000000000, 0.000000000000000000, 0.000000000000000000 ) ) ;
#8014 = CARTESIAN_POINT ( 'NONE',  ( -0.7188294034286043521, 37.49680007765647360, 2.395093729190366005 ) ) ;
#8015 = CARTESIAN_POINT ( 'NONE',  ( 4.000000000000000888, -20.49644878522406088, -4.990482410488609410 ) ) ;
#8016 = CARTESIAN_POINT ( 'NONE',  ( -3.518350579753630303, 33.12180007765646650, -1.080741659609802952 ) ) ;
#8017 = DIRECTION ( 'NONE',  ( 1.000000000000000000, 0.000000000000000000, -4.336808689942021680E-16 ) ) ;
#8018 = PRODUCT_CONTEXT ( 'NONE', #3466, 'mechanical' ) ;
#8019 = AXIS2_PLACEMENT_3D ( 'NONE', #10636, #7851, #16310 ) ;
#8020 = FACE_OUTER_BOUND ( 'NONE', #12578, .T. ) ;
#8021 = ORIENTED_EDGE ( 'NONE', *, *, #17741, .F. ) ;
#8022 = CARTESIAN_POINT ( 'NONE',  ( 4.243569643750003451, -19.41977419944868544, -7.724321858545000197 ) ) ;
#8023 = CARTESIAN_POINT ( 'NONE',  ( 1.027846397803542144, 26.24680007765648071, -3.346150245485522312 ) ) ;
#8024 = ORIENTED_EDGE ( 'NONE', *, *, #718, .F. ) ;
#8025 = CARTESIAN_POINT ( 'NONE',  ( 3.999999999999996447, -23.70025549648699936, -5.539674672087284257 ) ) ;
#8026 = CARTESIAN_POINT ( 'NONE',  ( 2.121784821875004390, -23.78282679764076590, -16.09115178578480254 ) ) ;
#8027 = CARTESIAN_POINT ( 'NONE',  ( -4.000000000000000000, 15.00000000000000355, 4.083367561434192880E-14 ) ) ;
#8028 = COLOUR_RGB ( '',0.8941176470588234615, 0.8941176470588234615, 0.8941176470588234615 ) ;
#8029 = CARTESIAN_POINT ( 'NONE',  ( 7.467138643671723308, -10.10634134916229598, 13.07939629701359152 ) ) ;
#8030 = EDGE_CURVE ( 'NONE', #12347, #10347, #6784, .T. ) ;
#8031 = CARTESIAN_POINT ( 'NONE',  ( -5.577813053751546416E-15, -24.09569370782749331, -3.156949689997003539 ) ) ;
#8032 = CARTESIAN_POINT ( 'NONE',  ( 4.243569643749996345, -27.83227623338511947, -11.19563964674263978 ) ) ;
#8033 = ORIENTED_EDGE ( 'NONE', *, *, #5346, .T. ) ;
#8034 = FACE_OUTER_BOUND ( 'NONE', #18065, .T. ) ;
#8035 = CARTESIAN_POINT ( 'NONE',  ( 3.999999999999996447, -24.28100163899737396, -6.369066117936657001 ) ) ;
#8036 = CARTESIAN_POINT ( 'NONE',  ( -3.500000000000000444, 35.49680007765648071, 0.05647727720536892260 ) ) ;
#8037 = ORIENTED_EDGE ( 'NONE', *, *, #4562, .F. ) ;
#8038 = ORIENTED_EDGE ( 'NONE', *, *, #17289, .T. ) ;
#8039 = CARTESIAN_POINT ( 'NONE',  ( 4.299564228933482956E-15, -19.02660638327880349, -9.865117096409875330 ) ) ;
#8040 = CARTESIAN_POINT ( 'NONE',  ( -0.05938372350918959958, 36.37819992234354771, 4.731580009072201776 ) ) ;
#8041 = DIRECTION ( 'NONE',  ( -1.000000000000000000, -0.000000000000000000, -0.000000000000000000 ) ) ;
#8042 = CARTESIAN_POINT ( 'NONE',  ( -0.7188294034286550893, 30.00319992234354416, -2.395093729190349130 ) ) ;
#8043 = ORIENTED_EDGE ( 'NONE', *, *, #4095, .T. ) ;
#8044 = CARTESIAN_POINT ( 'NONE',  ( 4.518350579753633411, 29.37180007765647716, 1.405661355842698468 ) ) ;
#8045 = CARTESIAN_POINT ( 'NONE',  ( 1.999999999999994449, -23.63520233397325399, -3.433610174171729312 ) ) ;
#8046 = ORIENTED_EDGE ( 'NONE', *, *, #11787, .T. ) ;
#8047 = FACE_OUTER_BOUND ( 'NONE', #17374, .T. ) ;
#8048 = CARTESIAN_POINT ( 'NONE',  ( -2.798362969681365886, 37.74680007765647360, 2.102939460078824929 ) ) ;
#8049 = CARTESIAN_POINT ( 'NONE',  ( 0.000000000000000000, 9.254131787996968228, 30.52396275209373044 ) ) ;
#8050 = AXIS2_PLACEMENT_3D ( 'NONE', #8528, #9920, #11311 ) ;
#8051 = CARTESIAN_POINT ( 'NONE',  ( 4.243569643749997233, -22.67008830622574322, -3.823271248141685508 ) ) ;
#8052 = AXIS2_PLACEMENT_3D ( 'NONE', #8616, #5936, #17090 ) ;
#8053 = CARTESIAN_POINT ( 'NONE',  ( -4.243569643750005227, -25.88570120251876361, -8.415642396436870953 ) ) ;
#8054 = PRODUCT_DEFINITION_FORMATION_WITH_SPECIFIED_SOURCE ( 'ANY', '', #1911, .NOT_KNOWN. ) ;
#8055 = DIRECTION ( 'NONE',  ( 0.000000000000000000, 0.000000000000000000, 1.000000000000000000 ) ) ;
#8056 = ORIENTED_EDGE ( 'NONE', *, *, #16997, .T. ) ;
#8057 = CARTESIAN_POINT ( 'NONE',  ( -8.500000000000005329, 10.00000000000000000, -18.49999999999999645 ) ) ;
#8058 = ORIENTED_EDGE ( 'NONE', *, *, #5520, .T. ) ;
#8059 = CARTESIAN_POINT ( 'NONE',  ( 2.864755990943222308, 35.50319992234354771, -2.011557305968548093 ) ) ;
#8060 = CARTESIAN_POINT ( 'NONE',  ( -2.864755990943222308, 19.25319992234354416, 2.011557305968548093 ) ) ;
#8061 = CARTESIAN_POINT ( 'NONE',  ( 4.243569643750003451, -18.61318233583002879, -6.572389296263599689 ) ) ;
#8062 = CARTESIAN_POINT ( 'NONE',  ( -2.055738996568313048, 33.24680007765648782, -1.423772053676023441 ) ) ;
#8063 = EDGE_CURVE ( 'NONE', #13521, #3191, #4128, .T. ) ;
#8064 = VECTOR ( 'NONE', #13426, 1000.000000000000000 ) ;
#8065 = CARTESIAN_POINT ( 'NONE',  ( 1.336863392178569754, 23.75319992234354771, 4.297206761780648421 ) ) ;
#8066 = AXIS2_PLACEMENT_3D ( 'NONE', #16222, #1955, #556 ) ;
#8067 = EDGE_CURVE ( 'NONE', #17010, #13521, #17171, .T. ) ;
#8068 = CARTESIAN_POINT ( 'NONE',  ( 2.000000000000004441, -21.48744557820235457, -12.44524936568625151 ) ) ;
#8069 = VERTEX_POINT ( 'NONE', #17219 ) ;
#8070 = ADVANCED_FACE ( 'NONE', ( #15367 ), #13299, .T. ) ;
#8071 = CARTESIAN_POINT ( 'NONE',  ( -4.000000000000004441, -27.46435086074564680, -10.91535996374058293 ) ) ;
#8072=STYLED_ITEM('',(#18396),#7822);
#8073 = CARTESIAN_POINT ( 'NONE',  ( -1.444289557196047014, 35.99680007765647360, -4.262301884875704161 ) ) ;
#8074 =( NAMED_UNIT ( * ) SI_UNIT ( $, .STERADIAN. ) SOLID_ANGLE_UNIT ( ) );
#8075 = EDGE_CURVE ( 'NONE', #16110, #15759, #16854, .T. ) ;
#8076 = CARTESIAN_POINT ( 'NONE',  ( 4.243569643750000786, -23.73894807732350998, -9.621251311363216985 ) ) ;
#8077 = CARTESIAN_POINT ( 'NONE',  ( -4.000000000000004441, -22.49574498014980151, -3.819455379080400004 ) ) ;
#8078 = DIRECTION ( 'NONE',  ( 0.000000000000000000, 0.000000000000000000, -1.000000000000000000 ) ) ;
#8079 = CARTESIAN_POINT ( 'NONE',  ( 8.500000000000019540, -1.201721234452885367, -20.49999999999998934 ) ) ;
#8080 = ORIENTED_EDGE ( 'NONE', *, *, #2647, .F. ) ;
#8081 = ORIENTED_EDGE ( 'NONE', *, *, #6147, .T. ) ;
#8082 = EDGE_CURVE ( 'NONE', #4334, #11008, #12408, .T. ) ;
#8083 = DIRECTION ( 'NONE',  ( 0.000000000000000000, 0.000000000000000000, 1.000000000000000000 ) ) ;
#8084 = LINE ( 'NONE', #1056, #13380 ) ;
#8085 = DIRECTION ( 'NONE',  ( 0.000000000000000000, 1.000000000000000000, 0.000000000000000000 ) ) ;
#8086 = ORIENTED_EDGE ( 'NONE', *, *, #10080, .T. ) ;
#8087 = CARTESIAN_POINT ( 'NONE',  ( 1.497042530366522461, 33.62819992234354771, 2.161531897785029965 ) ) ;
#8088 = CARTESIAN_POINT ( 'NONE',  ( 4.243569643750000786, -24.25516687003944938, -10.35848815122331068 ) ) ;
#8089 = CARTESIAN_POINT ( 'NONE',  ( 1.027846397803542144, 31.24680007765647716, -3.346150245485522312 ) ) ;
#8090 = CARTESIAN_POINT ( 'NONE',  ( 1.135272562821020070, 27.75319992234354416, -3.311245368580577164 ) ) ;
#8091 = CARTESIAN_POINT ( 'NONE',  ( 0.000000000000000000, 5.000000000000000000, 0.000000000000000000 ) ) ;
#8092 = FACE_OUTER_BOUND ( 'NONE', #12682, .T. ) ;
#8093 = AXIS2_PLACEMENT_3D ( 'NONE', #3964, #4148, #9616 ) ;
#8094 = CARTESIAN_POINT ( 'NONE',  ( -4.243569643750005227, -25.88570120251876361, -8.415642396436870953 ) ) ;
#8095 = DIRECTION ( 'NONE',  ( 0.000000000000000000, 0.000000000000000000, -1.000000000000000000 ) ) ;
#8096 = CARTESIAN_POINT ( 'NONE',  ( -4.518350579753632523, 20.62180007765647716, -1.405661355842698468 ) ) ;
#8097 = DIRECTION ( 'NONE',  ( 0.000000000000000000, 0.000000000000000000, -1.000000000000000000 ) ) ;
#8098 = DIRECTION ( 'NONE',  ( -0.000000000000000000, -1.000000000000000000, -0.000000000000000000 ) ) ;
#8099 = CARTESIAN_POINT ( 'NONE',  ( -2.121784821875005722, -24.51241577880647782, -4.318642500053448963 ) ) ;
#8100 = EDGE_LOOP ( 'NONE', ( #7988, #16976 ) ) ;
#8101 = AXIS2_PLACEMENT_3D ( 'NONE', #9932, #10201, #15603 ) ;
#8102 = CIRCLE ( 'NONE', #11643, 2.000000000000000444 ) ;
#8103 = DIRECTION ( 'NONE',  ( 0.000000000000000000, 0.000000000000000000, 1.000000000000000000 ) ) ;
#8104 = DIRECTION ( 'NONE',  ( -3.469446951953613696E-16, -0.000000000000000000, -1.000000000000000000 ) ) ;
#8105 = CARTESIAN_POINT ( 'NONE',  ( 0.8262555684461332373, 39.74680007765648071, 2.360188852285403982 ) ) ;
#8106 = CARTESIAN_POINT ( 'NONE',  ( 8.500000000000019540, 10.00000000000000000, -18.49999999999998934 ) ) ;
#8107 = CARTESIAN_POINT ( 'NONE',  ( 2.211161402132902243, 39.62180007765646650, 2.942372952327172442 ) ) ;
#8108 = DIRECTION ( 'NONE',  ( -0.000000000000000000, -1.000000000000000000, -0.000000000000000000 ) ) ;
#8109 = ITEM_DEFINED_TRANSFORMATION ( 'NONE', 'NONE', #367,  #16940 ) ;
#8110 = CYLINDRICAL_SURFACE ( 'NONE', #6898, 0.9999999999999991118 ) ;
#8111 = ORIENTED_EDGE ( 'NONE', *, *, #12876, .T. ) ;
#8112 = CARTESIAN_POINT ( 'NONE',  ( -5.330712181944246111E-15, -24.75231408233150887, -2.525507728232826210 ) ) ;
#8113 = UNCERTAINTY_MEASURE_WITH_UNIT (LENGTH_MEASURE( 1.000000000000000082E-05 ), #13700, 'distance_accuracy_value', 'NONE');
#8114 = CARTESIAN_POINT ( 'NONE',  ( 3.518350579753631191, 26.87180007765647360, 1.080741659609802285 ) ) ;
#8115 =( BOUNDED_CURVE ( )  B_SPLINE_CURVE ( 2, ( #14630, #2019, #3308, #17518, #4875, #8949, #7647, #8852, #434 ),
 .UNSPECIFIED., .F., .T. ) 
 B_SPLINE_CURVE_WITH_KNOTS ( ( 3, 2, 2, 2, 3 ),
 ( 0.3362068965517241437, 0.3390804597701149170, 0.3448275862068965747, 0.3505747126436781769, 0.3534482758620690057 ),
 .UNSPECIFIED. ) 
 CURVE ( )  GEOMETRIC_REPRESENTATION_ITEM ( )  RATIONAL_B_SPLINE_CURVE ( ( 0.9330127018922194093, 0.9330127018922200755, 1.000000000000000000, 0.8660254037844387076, 1.000000000000000000, 0.8660254037844387076, 1.000000000000000000, 0.9330127018922187432, 0.9330127018922194093 ) ) 
 REPRESENTATION_ITEM ( '' )  );
#8116 = ORIENTED_EDGE ( 'NONE', *, *, #2965, .F. ) ;
#8117 = PRODUCT ( 'MAS-178', 'MAS-178', '', ( #1662 ) ) ;
#8118 = DIRECTION ( 'NONE',  ( -3.469446951953613696E-16, -0.000000000000000000, -1.000000000000000000 ) ) ;
#8119 = DIRECTION ( 'NONE',  ( 0.000000000000000000, 0.8191520442889952403, -0.5735764363510413855 ) ) ;
#8120 = DIRECTION ( 'NONE',  ( 0.000000000000000000, -1.000000000000000000, 0.000000000000000000 ) ) ;
#8121 = CARTESIAN_POINT ( 'NONE',  ( 3.250767888004682415, -21.90484815091188509, -2.246271217071878379 ) ) ;
#8122 = CARTESIAN_POINT ( 'NONE',  ( -11.99999999999999822, 48.00000000000000000, 15.00000000000000000 ) ) ;
#8123 = CARTESIAN_POINT ( 'NONE',  ( 2.121784821874994176, -28.59914788780765704, -10.15510081561253664 ) ) ;
#8124 = VERTEX_POINT ( 'NONE', #2755 ) ;
#8125 = DIRECTION ( 'NONE',  ( -0.000000000000000000, -1.000000000000000000, -0.000000000000000000 ) ) ;
#8126 = CARTESIAN_POINT ( 'NONE',  ( 4.000000000000000888, -21.33530432409240163, -6.188492276268029890 ) ) ;
#8127 = CARTESIAN_POINT ( 'NONE',  ( 0.05938372350927906274, 37.37180007765645939, 3.680117784833935701 ) ) ;
#8128 = EDGE_LOOP ( 'NONE', ( #17895, #3121 ) ) ;
#8129 = ORIENTED_EDGE ( 'NONE', *, *, #10920, .T. ) ;
#8130 = CARTESIAN_POINT ( 'NONE',  ( 1.444289557195957086, 37.75319992234354771, -4.262301884875733471 ) ) ;
#8131 = DIRECTION ( 'NONE',  ( 0.000000000000000000, 0.000000000000000000, 1.000000000000000000 ) ) ;
#8132 = CARTESIAN_POINT ( 'NONE',  ( 1.989345975306457071, 31.00319992234355126, 1.515154207786300500 ) ) ;
#8133 = VECTOR ( 'NONE', #15814, 1000.000000000000000 ) ;
#8134 = ORIENTED_EDGE ( 'NONE', *, *, #11225, .T. ) ;
#8135 = CARTESIAN_POINT ( 'NONE',  ( -4.243569643750004339, -27.43435758066658181, -10.62735291601715382 ) ) ;
#8136 = CARTESIAN_POINT ( 'NONE',  ( -1.336863392178478716, 22.49680007765647360, 4.297206761780677731 ) ) ;
#8137 = EDGE_CURVE ( 'NONE', #1200, #9609, #8908, .T. ) ;
#8138 = CARTESIAN_POINT ( 'NONE',  ( -1.999999999999996225, -18.34711458918039995, -7.960391923204007014 ) ) ;
#8139 = VERTEX_POINT ( 'NONE', #11345 ) ;
#8140 = CARTESIAN_POINT ( 'NONE',  ( 0.000000000000000000, 9.254131787996968228, 30.52396275209373044 ) ) ;
#8141 = DIRECTION ( 'NONE',  ( -0.000000000000000000, -1.000000000000000000, -0.000000000000000000 ) ) ;
#8142 = DIRECTION ( 'NONE',  ( 0.000000000000000000, 0.000000000000000000, 1.000000000000000000 ) ) ;
#8143 = CARTESIAN_POINT ( 'NONE',  ( 0.000000000000000000, 3.000000000000000000, 2.499999999999999556 ) ) ;
#8144 = CARTESIAN_POINT ( 'NONE',  ( -2.121784821875005722, -25.31900764242513091, -5.470575062334849470 ) ) ;
#8145 = CARTESIAN_POINT ( 'NONE',  ( -15.00000000000000178, 13.00000000000000178, -25.00000000000000355 ) ) ;
#8146 = ORIENTED_EDGE ( 'NONE', *, *, #12602, .F. ) ;
#8147 = CARTESIAN_POINT ( 'NONE',  ( -2.000000000000005773, -27.61438886186354225, -9.116477482433401391 ) ) ;
#8148 = VECTOR ( 'NONE', #11143, 1000.000000000000000 ) ;
#8149 = CYLINDRICAL_SURFACE ( 'NONE', #4804, 0.9999999999999991118 ) ;
#8150 = CARTESIAN_POINT ( 'NONE',  ( -1.027846397803541700, 17.49680007765647716, 3.346150245485522312 ) ) ;
#8151 =( NAMED_UNIT ( * ) PLANE_ANGLE_UNIT ( ) SI_UNIT ( $, .RADIAN. ) );
#8152 = EDGE_LOOP ( 'NONE', ( #13396, #13900, #9530, #6124 ) ) ;
#8153 = CARTESIAN_POINT ( 'NONE',  ( 1.135272562821020070, 37.75319992234354061, -3.311245368580577164 ) ) ;
#8154 = CARTESIAN_POINT ( 'NONE',  ( 3.518350579753606322, 18.12819992234354416, -1.080741659609876892 ) ) ;
#8155 = CARTESIAN_POINT ( 'NONE',  ( -2.121784821874996396, -16.77085486324927999, -6.077018044351843784 ) ) ;
#8156 = CARTESIAN_POINT ( 'NONE',  ( 1.593127413382998903, 32.12180007765648071, 2.091722143975139669 ) ) ;
#8157 = CARTESIAN_POINT ( 'NONE',  ( 4.499999999999999112, 25.75319992234354771, 0.05647727720528474687 ) ) ;
#8158 = CARTESIAN_POINT ( 'NONE',  ( -3.999999999999997335, -23.14312172474173224, -12.79664100063768650 ) ) ;
#8159 = ORIENTED_EDGE ( 'NONE', *, *, #6799, .T. ) ;
#8160 = CARTESIAN_POINT ( 'NONE',  ( 2.343145750507618530, -3.999999999999991562, 11.59510085796835099 ) ) ;
#8161 = CARTESIAN_POINT ( 'NONE',  ( 0.05938372350927906274, 24.87180007765647005, 3.680117784833935701 ) ) ;
#8162 = AXIS2_PLACEMENT_3D ( 'NONE', #15331, #15147, #9746 ) ;
#8163 = CARTESIAN_POINT ( 'NONE',  ( -8.999999999999996447, -10.00000000000000000, -3.713574246709372417 ) ) ;
#8164 = CARTESIAN_POINT ( 'NONE',  ( -2.121784821875005722, -27.35161913874413386, -8.373445119283974947 ) ) ;
#8165 = CIRCLE ( 'NONE', #1362, 2.200000000000000622 ) ;
#8166 = CARTESIAN_POINT ( 'NONE',  ( 4.299564228933482956E-15, -17.41342265533655009, -7.561251970840314307 ) ) ;
#8167 = ADVANCED_FACE ( 'NONE', ( #5519 ), #11164, .T. ) ;
#8168 = EDGE_CURVE ( 'NONE', #4710, #6649, #9684, .T. ) ;
#8169 = CYLINDRICAL_SURFACE ( 'NONE', #914, 4.000000000000001776 ) ;
#8170 = CARTESIAN_POINT ( 'NONE',  ( 13.00000000000000178, 13.00000000000000178, 0.000000000000000000 ) ) ;
#8171 = ORIENTED_EDGE ( 'NONE', *, *, #13976, .F. ) ;
#8172 = ORIENTED_EDGE ( 'NONE', *, *, #11787, .F. ) ;
#8173 = CARTESIAN_POINT ( 'NONE',  ( 8.000000000000001776, 20.99999999999999289, -2.500000000000002220 ) ) ;
#8174 = FACE_OUTER_BOUND ( 'NONE', #1527, .T. ) ;
#8175 = CARTESIAN_POINT ( 'NONE',  ( -4.648177544792955347E-16, -30.09673717385520675, -11.72732795437737785 ) ) ;
#8176 = CARTESIAN_POINT ( 'NONE',  ( -10.00000000000000000, 40.79999999999999716, 2.499999999999998224 ) ) ;
#8177 = ORIENTED_EDGE ( 'NONE', *, *, #16181, .F. ) ;
#8178 = CARTESIAN_POINT ( 'NONE',  ( -0.7188294034286550893, 32.50319992234354771, -2.395093729190349130 ) ) ;
#8179 = CARTESIAN_POINT ( 'NONE',  ( 4.730628863548789710E-15, -19.91864238692259903, -12.70826957775434352 ) ) ;
#8180 = CARTESIAN_POINT ( 'NONE',  ( -3.518350579753630747, 28.12180007765647360, -1.080741659609802729 ) ) ;
#8181 = CARTESIAN_POINT ( 'NONE',  ( -2.211161402132839182, 26.62819992234353705, 2.942372952327218627 ) ) ;
#8182 = DIRECTION ( 'NONE',  ( -0.000000000000000000, -0.5735764363510414965, -0.8191520442889950182 ) ) ;
#8183 = TOROIDAL_SURFACE ( 'NONE', #8765, 9.000000000000001776, 0.9999999999999991118 ) ;
#8184 = DIRECTION ( 'NONE',  ( 1.000000000000000000, 0.000000000000000000, -4.336808689942021680E-16 ) ) ;
#8185 = CARTESIAN_POINT ( 'NONE',  ( 2.121784821874994176, -27.34086458056255964, -8.358086018453551702 ) ) ;
#8186 = CARTESIAN_POINT ( 'NONE',  ( -0.4504932947034102630, -10.00000000000000178, -12.59063537424963997 ) ) ;
#8187 = ADVANCED_FACE ( 'NONE', ( #8301 ), #15718, .T. ) ;
#8188 = APPLICATION_CONTEXT ( 'automotive_design' ) ;
#8189 = CARTESIAN_POINT ( 'NONE',  ( -4.000000000000000888, -20.69003083319747205, -5.266946226442914991 ) ) ;
#8190 = EDGE_CURVE ( 'NONE', #6514, #16507, #3012, .T. ) ;
#8191 = CARTESIAN_POINT ( 'NONE',  ( -3.500000000000000444, 15.00000000000001243, 3.664603343001004987E-14 ) ) ;
#8192 = AXIS2_PLACEMENT_3D ( 'NONE', #1067, #791, #5043 ) ;
#8193 = CARTESIAN_POINT ( 'NONE',  ( 4.243569643749996345, -24.21874468437355432, -6.034981767721971480 ) ) ;
#8194 = DIRECTION ( 'NONE',  ( -1.000000000000000000, -0.000000000000000000, -0.000000000000000000 ) ) ;
#8195 = CARTESIAN_POINT ( 'NONE',  ( 3.579096709490575479E-14, -24.41833045397989821, -3.617722715916328546 ) ) ;
#8196 = CARTESIAN_POINT ( 'NONE',  ( -2.481649420246374138, 37.87180007765647360, 0.8687765177876256573 ) ) ;
#8197 = CARTESIAN_POINT ( 'NONE',  ( 3.579096709490575479E-14, -23.83758431146952361, -2.788331270066955359 ) ) ;
#8198 = CARTESIAN_POINT ( 'NONE',  ( 1.027846397803542144, 36.24680007765648071, -3.346150245485522312 ) ) ;
#8199 = MANIFOLD_SOLID_BREP ( 'LPattern6[7]', #226 ) ;
#8200 = CARTESIAN_POINT ( 'NONE',  ( -1.071796769724494114, -29.85015447821607637, -11.37517136910324744 ) ) ;
#8201 = ITEM_DEFINED_TRANSFORMATION ( 'NONE', 'NONE', #2742,  #16940 ) ;
#8202 = DIRECTION ( 'NONE',  ( -0.000000000000000000, -1.000000000000000000, -0.000000000000000000 ) ) ;
#8203 = ORIENTED_EDGE ( 'NONE', *, *, #5704, .F. ) ;
#8204 = CARTESIAN_POINT ( 'NONE',  ( 4.243569643749997233, -23.99289896256033572, -5.712440650283180155 ) ) ;
#8205 = CARTESIAN_POINT ( 'NONE',  ( 2.211161402132902243, 22.12180007765648071, 2.942372952327172442 ) ) ;
#8206 = VECTOR ( 'NONE', #260, 1000.000000000000000 ) ;
#8207 = CYLINDRICAL_SURFACE ( 'NONE', #2940, 4.000000000000000000 ) ;
#8208 = CARTESIAN_POINT ( 'NONE',  ( -2.121784821875005722, -29.41649430960788081, -11.32239247872435506 ) ) ;
#8209 = DIRECTION ( 'NONE',  ( -0.000000000000000000, -1.000000000000000000, -0.000000000000000000 ) ) ;
#8210 = DIRECTION ( 'NONE',  ( -3.469446951953613696E-16, -0.000000000000000000, -1.000000000000000000 ) ) ;
#8211 = DIRECTION ( 'NONE',  ( 0.000000000000000000, 0.000000000000000000, -1.000000000000000000 ) ) ;
#8212 = CARTESIAN_POINT ( 'NONE',  ( -5.330712181944245322E-15, -30.14034773130410372, -10.22041724427257137 ) ) ;
#8213 = ORIENTED_EDGE ( 'NONE', *, *, #17316, .T. ) ;
#8214 = DIRECTION ( 'NONE',  ( 0.000000000000000000, 0.000000000000000000, -1.000000000000000000 ) ) ;
#8215 = CARTESIAN_POINT ( 'NONE',  ( -2.000000000000005773, -25.03329489828385590, -5.430293283132924032 ) ) ;
#8216 = PRESENTATION_LAYER_ASSIGNMENT (  '', '', ( #2021 ) ) ;
#8217 = CARTESIAN_POINT ( 'NONE',  ( 1.593127413382998903, 17.12180007765648426, 2.091722143975139669 ) ) ;
#8218 = VECTOR ( 'NONE', #4309, 1000.000000000000000 ) ;
#8219 = ORIENTED_EDGE ( 'NONE', *, *, #2090, .T. ) ;
#8220 = CARTESIAN_POINT ( 'NONE',  ( 1.999999999999994449, -28.34569881821112602, -10.16089633890186761 ) ) ;
#8221 =( LENGTH_UNIT ( ) NAMED_UNIT ( * ) SI_UNIT ( .MILLI., .METRE. ) );
#8222 = CARTESIAN_POINT ( 'NONE',  ( 2.733110507866328920, 31.12819992234354416, 3.862833514489095510 ) ) ;
#8223 = CARTESIAN_POINT ( 'NONE',  ( -1.734723475976807094E-15, 18.79999999999999361, -11.50000000000000178 ) ) ;
#8224 = CARTESIAN_POINT ( 'NONE',  ( 2.055738996568281518, 28.00319992234354771, -1.423772053676066518 ) ) ;
#8225 =( BOUNDED_CURVE ( )  B_SPLINE_CURVE ( 2, ( #7787, #6403, #16062, #13531, #12049, #3708, #17830, #4830, #3354 ),
 .UNSPECIFIED., .F., .T. ) 
 B_SPLINE_CURVE_WITH_KNOTS ( ( 3, 2, 2, 2, 3 ),
 ( 0.9741379310344827624, 0.9770114942528735913, 0.9827586206896551380, 0.9885057471264367956, 0.9913793103448276245 ),
 .UNSPECIFIED. ) 
 CURVE ( )  GEOMETRIC_REPRESENTATION_ITEM ( )  RATIONAL_B_SPLINE_CURVE ( ( 0.9330127018922194093, 0.9330127018922194093, 1.000000000000000000, 0.8660254037844387076, 1.000000000000000000, 0.8660254037844387076, 1.000000000000000000, 0.9330127018922180770, 0.9330127018922194093 ) ) 
 REPRESENTATION_ITEM ( '' )  );
#8226 = ORIENTED_EDGE ( 'NONE', *, *, #802, .F. ) ;
#8227 = CARTESIAN_POINT ( 'NONE',  ( -5.330712181944246111E-15, -30.17261140584885126, -10.26649454676382867 ) ) ;
#8228 = CARTESIAN_POINT ( 'NONE',  ( -2.733110507866247652, 27.62180007765647716, 3.862833514489154574 ) ) ;
#8229 = CARTESIAN_POINT ( 'NONE',  ( -3.999999999999997335, -19.01337138301423479, -6.898746281756922727 ) ) ;
#8230 = ORIENTED_EDGE ( 'NONE', *, *, #12650, .T. ) ;
#8231 = CIRCLE ( 'NONE', #241, 2.499999999999999556 ) ;
#8232 = DIRECTION ( 'NONE',  ( -0.000000000000000000, -1.000000000000000000, -0.000000000000000000 ) ) ;
#8233 = ADVANCED_FACE ( 'NONE', ( #1538 ), #331, .F. ) ;
#8234 = AXIS2_PLACEMENT_3D ( 'NONE', #1325, #2537, #15242 ) ;
#8235 = DIRECTION ( 'NONE',  ( -0.000000000000000000, -0.5735764363510414965, -0.8191520442889950182 ) ) ;
#8236 = CARTESIAN_POINT ( 'NONE',  ( 0.000000000000000000, 5.977523610840987267, 32.81826849749789687 ) ) ;
#8237 = ADVANCED_FACE ( 'NONE', ( #6252 ), #17317, .F. ) ;
#8238 = CARTESIAN_POINT ( 'NONE',  ( -9.000000000000003553, 20.99999999999999289, -2.500000000000001776 ) ) ;
#8239 = CARTESIAN_POINT ( 'NONE',  ( 2.121784821874994176, -26.05031759877271469, -6.514993918803313910 ) ) ;
#8240 = EDGE_CURVE ( 'NONE', #4607, #18076, #50, .T. ) ;
#8241 = ORIENTED_EDGE ( 'NONE', *, *, #4555, .T. ) ;
#8242 = DIRECTION ( 'NONE',  ( -1.000000000000000000, 0.000000000000000000, 4.336808689942021680E-16 ) ) ;
#8243 = EDGE_CURVE ( 'NONE', #159, #9984, #14802, .T. ) ;
#8244 = EDGE_LOOP ( 'NONE', ( #9413, #6544, #6426, #12500 ) ) ;
#8245 = CARTESIAN_POINT ( 'NONE',  ( 4.000000000000000888, -24.43261708038802382, -10.61191331542860183 ) ) ;
#8246 = LINE ( 'NONE', #2701, #14585 ) ;
#8247 = CARTESIAN_POINT ( 'NONE',  ( -3.518350579753630303, 15.62180007765647716, -1.080741659609802952 ) ) ;
#8248 = PRODUCT_DEFINITION_SHAPE ( 'NONE', 'NONE',  #18380 ) ;
#8249 = ORIENTED_EDGE ( 'NONE', *, *, #1449, .T. ) ;
#8250 = PRESENTATION_LAYER_ASSIGNMENT (  '', '', ( #12384 ) ) ;
#8251 = CARTESIAN_POINT ( 'NONE',  ( 3.500000000000000444, 38.25319992234354061, 0.05647727720529520379 ) ) ;
#8252 = CARTESIAN_POINT ( 'NONE',  ( -3.518350579753606322, 21.87819992234354771, 1.080741659609877781 ) ) ;
#8253 = CIRCLE ( 'NONE', #1704, 0.9999999999999991118 ) ;
#8254 = CARTESIAN_POINT ( 'NONE',  ( -2.121784821874996396, -17.28707365596521939, -6.814254884211938368 ) ) ;
#8255 = CARTESIAN_POINT ( 'NONE',  ( 2.055738996568313048, 26.99680007765647716, 1.423772053676023441 ) ) ;
#8256 = CARTESIAN_POINT ( 'NONE',  ( 1.444289557195957086, 25.25319992234354771, -4.262301884875733471 ) ) ;
#8257 = UNCERTAINTY_MEASURE_WITH_UNIT (LENGTH_MEASURE( 1.000000000000000082E-05 ), #8924, 'distance_accuracy_value', 'NONE');
#8258 = CARTESIAN_POINT ( 'NONE',  ( -2.000000000000005773, -27.54986151206910350, -9.024322876444124120 ) ) ;
#8259 = ORIENTED_EDGE ( 'NONE', *, *, #3999, .T. ) ;
#8260 = DIRECTION ( 'NONE',  ( 0.000000000000000000, 0.000000000000000000, 1.000000000000000000 ) ) ;
#8261 = CARTESIAN_POINT ( 'NONE',  ( 3.481649420246369697, 19.12180007765648071, -1.193696214020541824 ) ) ;
#8262 = CARTESIAN_POINT ( 'NONE',  ( 0.000000000000000000, 5.977523610840987267, 32.81826849749789687 ) ) ;
#8263 = AXIS2_PLACEMENT_3D ( 'NONE', #12199, #4883, #10535 ) ;
#8264 = CARTESIAN_POINT ( 'NONE',  ( -4.243569643750004339, -24.56289054618417111, -6.526472994295373198 ) ) ;
#8265 = EDGE_CURVE ( 'NONE', #18266, #16267, #2101, .T. ) ;
#8266 = DIRECTION ( 'NONE',  ( -0.000000000000000000, 0.000000000000000000, 1.000000000000000000 ) ) ;
#8267 = ADVANCED_FACE ( 'NONE', ( #8841 ), #2533, .T. ) ;
#8268 = VERTEX_POINT ( 'NONE', #5968 ) ;
#8269 = ORIENTED_EDGE ( 'NONE', *, *, #17528, .F. ) ;
#8270 = CYLINDRICAL_SURFACE ( 'NONE', #4993, 0.9999999999999991118 ) ;
#8271 = DIRECTION ( 'NONE',  ( -0.000000000000000000, -0.5735764363510414965, -0.8191520442889950182 ) ) ;
#8272 = CARTESIAN_POINT ( 'NONE',  ( 0.000000000000000000, 5.000000000000000000, -2.499999999999999556 ) ) ;
#8273 = CARTESIAN_POINT ( 'NONE',  ( 1.071796769724476128, -19.55435187671356800, -10.61881577092589524 ) ) ;
#8274 = ORIENTED_EDGE ( 'NONE', *, *, #18132, .F. ) ;
#8275 = CARTESIAN_POINT ( 'NONE',  ( 2.055738996568281518, 38.00319992234354061, -1.423772053676066518 ) ) ;
#8276 = AXIS2_PLACEMENT_3D ( 'NONE', #11417, #17205, #8456 ) ;
#8277 = CARTESIAN_POINT ( 'NONE',  ( -5.330712181944245322E-15, -28.07547256044035322, -7.271469884832189479 ) ) ;
#8278 = CARTESIAN_POINT ( 'NONE',  ( -3.481649420246369697, 32.87180007765645939, 1.193696214020542490 ) ) ;
#8279 = AXIS2_PLACEMENT_3D ( 'NONE', #6845, #1475, #8770 ) ;
#8280 = CARTESIAN_POINT ( 'NONE',  ( 3.481649420246394122, 25.87819992234354771, 1.193696214020467439 ) ) ;
#8281 = CARTESIAN_POINT ( 'NONE',  ( -1.734723475976807094E-15, 29.79999999999999716, -2.500000000000000000 ) ) ;
#8282 = CARTESIAN_POINT ( 'NONE',  ( -10.00000000000000000, 34.19999999999999574, 2.499999999999998224 ) ) ;
#8283 = CARTESIAN_POINT ( 'NONE',  ( 2.121784821874994176, -26.56653639148865409, -7.252230758663410271 ) ) ;
#8284 = DIRECTION ( 'NONE',  ( 0.000000000000000000, 1.000000000000000000, -1.478898702612462246E-15 ) ) ;
#8285 = VECTOR ( 'NONE', #10608, 1000.000000000000000 ) ;
#8286 = CARTESIAN_POINT ( 'NONE',  ( 0.000000000000000000, 0.000000000000000000, 0.000000000000000000 ) ) ;
#8287 = CARTESIAN_POINT ( 'NONE',  ( -4.000000000000000888, -20.94814022955544175, -5.635564646372960951 ) ) ;
#8288 = CARTESIAN_POINT ( 'NONE',  ( -5.330712181944245322E-15, -26.01059738957660272, -4.322522525391808479 ) ) ;
#8289 = CARTESIAN_POINT ( 'NONE',  ( 4.000000000000000000, 0.000000000000000000, 0.000000000000000000 ) ) ;
#8290 = FILL_AREA_STYLE_COLOUR ( '', #17731 ) ;
#8291 = CARTESIAN_POINT ( 'NONE',  ( -0.7188294034286550893, 15.00319992234354594, -2.395093729190349130 ) ) ;
#8292 = CARTESIAN_POINT ( 'NONE',  ( 0.05938372350927906967, 34.87180007765646650, 3.680117784833935701 ) ) ;
#8293 = DIRECTION ( 'NONE',  ( 0.000000000000000000, 0.000000000000000000, 1.000000000000000000 ) ) ;
#8294 = CARTESIAN_POINT ( 'NONE',  ( -1.064077915893153703, 15.00000000000000178, -3.362852706530892632 ) ) ;
#8295 = EDGE_CURVE ( 'NONE', #8139, #8268, #14418, .T. ) ;
#8296 = ORIENTED_EDGE ( 'NONE', *, *, #14411, .T. ) ;
#8297 = CARTESIAN_POINT ( 'NONE',  ( 4.243569643750000786, -21.19011778828857118, -5.981144414553994260 ) ) ;
#8298 = CARTESIAN_POINT ( 'NONE',  ( -2.798362969681365886, 25.24680007765647716, 2.102939460078824929 ) ) ;
#8299 = EDGE_CURVE ( 'NONE', #3027, #4548, #5452, .T. ) ;
#8300 = EDGE_CURVE ( 'NONE', #1591, #1834, #14637, .T. ) ;
#8301 = FACE_OUTER_BOUND ( 'NONE', #18012, .T. ) ;
#8302 = CARTESIAN_POINT ( 'NONE',  ( 4.243569643749997233, -28.34849502610105176, -11.93287648660273526 ) ) ;
#8303 = PLANE ( 'NONE',  #13810 ) ;
#8304 = EDGE_CURVE ( 'NONE', #15374, #2571, #7819, .T. ) ;
#8305 = DIRECTION ( 'NONE',  ( -4.915049848600951133E-16, 0.000000000000000000, -1.000000000000000000 ) ) ;
#8306 = DIRECTION ( 'NONE',  ( -0.000000000000000000, -1.000000000000000000, -0.000000000000000000 ) ) ;
#8307 = CARTESIAN_POINT ( 'NONE',  ( 4.243569643750000786, -25.54571385182929077, -12.20158025087355114 ) ) ;
#8308 = ORIENTED_EDGE ( 'NONE', *, *, #16301, .F. ) ;
#8309 = CARTESIAN_POINT ( 'NONE',  ( -3.999999999999997335, -21.59446534659392114, -10.58493048105740009 ) ) ;
#8310 = CARTESIAN_POINT ( 'NONE',  ( -3.999999999999997335, -19.85222692188257554, -8.096756147536344983 ) ) ;
#8311 = VECTOR ( 'NONE', #15192, 1000.000000000000000 ) ;
#8312 = CARTESIAN_POINT ( 'NONE',  ( 1.135272562821090458, 37.24680007765648071, 3.311245368580554072 ) ) ;
#8313 = ORIENTED_EDGE ( 'NONE', *, *, #3073, .T. ) ;
#8314 = CARTESIAN_POINT ( 'NONE',  ( -3.673772985318219053, 15.74680007765647716, -2.599342558260952174 ) ) ;
#8315 = LINE ( 'NONE', #15384, #10744 ) ;
#8316 = CARTESIAN_POINT ( 'NONE',  ( -2.055738996568281518, 39.25319992234354771, 1.423772053676066962 ) ) ;
#8317 = ORIENTED_EDGE ( 'NONE', *, *, #4973, .F. ) ;
#8318 = CARTESIAN_POINT ( 'NONE',  ( -4.243569643750004339, -27.17624818430860500, -10.25873449608710786 ) ) ;
#8319 = CARTESIAN_POINT ( 'NONE',  ( 4.481649420246366589, 24.12180007765647716, -1.518615910253458212 ) ) ;
#8320 = CARTESIAN_POINT ( 'NONE',  ( -4.243569643750005227, -28.98301395881438580, -12.83906343559744201 ) ) ;
#8321 = MANIFOLD_SOLID_BREP ( 'Hex', #183 ) ;
#8322 = ORIENTED_EDGE ( 'NONE', *, *, #14092, .T. ) ;
#8323 = LINE ( 'NONE', #2598, #7678 ) ;
#8324 = CARTESIAN_POINT ( 'NONE',  ( -4.000000000000000888, -24.04545298585106394, -10.05898568553353378 ) ) ;
#8325 = DIRECTION ( 'NONE',  ( -0.000000000000000000, 1.000000000000000000, -0.000000000000000000 ) ) ;
#8326 = CARTESIAN_POINT ( 'NONE',  ( -5.000000000000001776, 0.000000000000000000, -4.999999999999999112 ) ) ;
#8327 = CARTESIAN_POINT ( 'NONE',  ( 4.730628863548789710E-15, -18.40224968331953548, -10.54263636066531085 ) ) ;
#8328 = VERTEX_POINT ( 'NONE', #16904 ) ;
#8329 = CARTESIAN_POINT ( 'NONE',  ( 8.499999999999992895, 15.00000000000000000, 20.49999999999999645 ) ) ;
#8330 = EDGE_LOOP ( 'NONE', ( #16677, #45, #581, #12119 ) ) ;
#8331 = CARTESIAN_POINT ( 'NONE',  ( -4.000000000000000888, -24.81978117492496949, -11.16484094532367699 ) ) ;
#8332 = LINE ( 'NONE', #3795, #6014 ) ;
#8333 = FACE_OUTER_BOUND ( 'NONE', #7668, .T. ) ;
#8334 =( NAMED_UNIT ( * ) SI_UNIT ( $, .STERADIAN. ) SOLID_ANGLE_UNIT ( ) );
#8335 = COLOUR_RGB ( '',0.8941176470588234615, 0.8941176470588234615, 0.8941176470588234615 ) ;
#8336 = CARTESIAN_POINT ( 'NONE',  ( 2.829195390882724759, 15.37819992234354594, -3.793023760679264278 ) ) ;
#8337 = CARTESIAN_POINT ( 'NONE',  ( 2.211161402132839182, 20.37819992234354416, -2.942372952327217739 ) ) ;
#8338 = CARTESIAN_POINT ( 'NONE',  ( 4.000000000000000888, -25.46505466581989907, -12.08638699514879455 ) ) ;
#8339 = CARTESIAN_POINT ( 'NONE',  ( -2.055738996568313048, 28.24680007765648071, -1.423772053676023441 ) ) ;
#8340 = CARTESIAN_POINT ( 'NONE',  ( -1.336863392178569088, 25.00319992234354771, -4.297206761780648421 ) ) ;
#8341 = CARTESIAN_POINT ( 'NONE',  ( 4.000000000000000888, -24.88430852330952447, -11.25699554929942003 ) ) ;
#8342 = ORIENTED_EDGE ( 'NONE', *, *, #6882, .T. ) ;
#8343 = CIRCLE ( 'NONE', #3615, 8.000000000000001776 ) ;
#8344 = CARTESIAN_POINT ( 'NONE',  ( -1.661723472263481630E-14, -21.54317299706404754, -13.45914668972107897 ) ) ;
#8345 = AXIS2_PLACEMENT_3D ( 'NONE', #6611, #16733, #15148 ) ;
#8346 = CARTESIAN_POINT ( 'NONE',  ( 0.05938372350927906274, 19.87180007765648426, 3.680117784833935701 ) ) ;
#8347 = ADVANCED_FACE ( 'NONE', ( #2622 ), #3204, .F. ) ;
#8348 = DIRECTION ( 'NONE',  ( -3.469446951953613696E-16, -0.000000000000000000, -1.000000000000000000 ) ) ;
#8349 = AXIS2_PLACEMENT_3D ( 'NONE', #11541, #7556, #17519 ) ;
#8350 = CARTESIAN_POINT ( 'NONE',  ( 4.243569643749997233, -24.99307287344746342, -7.140837027512114688 ) ) ;
#8351 = MANIFOLD_SOLID_BREP ( 'LPattern6[9]', #10285 ) ;
#8352 = CARTESIAN_POINT ( 'NONE',  ( -9.000000000000001776, 18.79999999999999361, 2.499999999999995559 ) ) ;
#8353 = FACE_OUTER_BOUND ( 'NONE', #9090, .T. ) ;
#8354 = VERTEX_POINT ( 'NONE', #1409 ) ;
#8355 = VERTEX_POINT ( 'NONE', #1319 ) ;
#8356 = CARTESIAN_POINT ( 'NONE',  ( -0.05938372350927861171, 26.12180007765647005, -3.680117784833935701 ) ) ;
#8357 = CARTESIAN_POINT ( 'NONE',  ( -1.734723475976807094E-15, 29.79999999999999716, -11.50000000000000178 ) ) ;
#8358 = AXIS2_PLACEMENT_3D ( 'NONE', #1954, #16041, #457 ) ;
#8359 = CARTESIAN_POINT ( 'NONE',  ( -5.577813053751546416E-15, -24.67643985033786791, -3.986341135846375838 ) ) ;
#8360 = VERTEX_POINT ( 'NONE', #15322 ) ;
#8361 = CIRCLE ( 'NONE', #6886, 0.4000000000000006883 ) ;
#8362 = CARTESIAN_POINT ( 'NONE',  ( -1.593127413382952939, 36.62819992234354771, 2.091722143975172532 ) ) ;
#8363 = CARTESIAN_POINT ( 'NONE',  ( 4.243569643750003451, -21.45238569576768484, -10.62719191549412656 ) ) ;
#8364 = CARTESIAN_POINT ( 'NONE',  ( -3.500000000000000444, 32.99680007765648071, 0.05647727720536892260 ) ) ;
#8365 = CARTESIAN_POINT ( 'NONE',  ( 3.518350579753605434, 30.62819992234353705, -1.080741659609877114 ) ) ;
#8366 = DIRECTION ( 'NONE',  ( -1.000000000000000000, -0.000000000000000000, -0.000000000000000000 ) ) ;
#8367 = DIRECTION ( 'NONE',  ( -1.214671430232282197E-14, -0.8191520442889843601, 0.5735764363510568176 ) ) ;
#8368 = CARTESIAN_POINT ( 'NONE',  ( -2.121784821875005722, -26.60955462421497586, -7.313667161985088150 ) ) ;
#8369 = ADVANCED_FACE ( 'NONE', ( #3811 ), #1136, .T. ) ;
#8370 = AXIS2_PLACEMENT_3D ( 'NONE', #6810, #5237, #8017 ) ;
#8371 = DIRECTION ( 'NONE',  ( -0.000000000000000000, -0.000000000000000000, 1.000000000000000000 ) ) ;
#8372 = DIRECTION ( 'NONE',  ( -4.915049848600951133E-16, 0.000000000000000000, -1.000000000000000000 ) ) ;
#8373 = DIRECTION ( 'NONE',  ( -1.000000000000000000, -0.000000000000000000, -0.000000000000000000 ) ) ;
#8374 = CARTESIAN_POINT ( 'NONE',  ( 4.243569643750003451, -19.64561992126190049, -8.046862975983790633 ) ) ;
#8375 = FACE_BOUND ( 'NONE', #14935, .T. ) ;
#8376 = CARTESIAN_POINT ( 'NONE',  ( -0.8262555684461330152, 38.49680007765647360, -2.360188852285403982 ) ) ;
#8377 = CARTESIAN_POINT ( 'NONE',  ( -8.000000000000001776, 13.00000000000000178, -2.499999999999997335 ) ) ;
#8378 = CARTESIAN_POINT ( 'NONE',  ( 1.533898589781675205E-14, -28.03186200299146336, -8.778380594936995962 ) ) ;
#8379 = CIRCLE ( 'NONE', #1897, 0.9999999999999991118 ) ;
#8380 = CARTESIAN_POINT ( 'NONE',  ( -9.570896052262728659, -9.974056209534193584, -0.5937313284778471534 ) ) ;
#8381 = VERTEX_POINT ( 'NONE', #6952 ) ;
#8382 = CARTESIAN_POINT ( 'NONE',  ( 2.121784821874994176, -24.50166122062490359, -4.303283399223027494 ) ) ;
#8383 = CARTESIAN_POINT ( 'NONE',  ( 2.798362969681366330, 33.99680007765648071, -2.102939460078824929 ) ) ;
#8384 = DIRECTION ( 'NONE',  ( 1.000000000000000000, 0.000000000000000000, -4.336808689942021680E-16 ) ) ;
#8385 = CYLINDRICAL_SURFACE ( 'NONE', #11215, 4.000000000000000000 ) ;
#8386 = CARTESIAN_POINT ( 'NONE',  ( 8.499999999999992895, 15.00000000000000000, 20.49999999999999645 ) ) ;
#8387 = AXIS2_PLACEMENT_3D ( 'NONE', #5961, #14228, #12827 ) ;
#8388 = DIRECTION ( 'NONE',  ( 0.000000000000000000, 1.000000000000000000, -1.502314598737159031E-16 ) ) ;
#8389 = DIRECTION ( 'NONE',  ( -1.000000000000000000, -0.000000000000000000, -0.000000000000000000 ) ) ;
#8390 = CARTESIAN_POINT ( 'NONE',  ( -2.121784821875005722, -29.15838491324991466, -10.95377405879430910 ) ) ;
#8391 = EDGE_CURVE ( 'NONE', #6288, #2227, #7150, .T. ) ;
#8392 = EDGE_LOOP ( 'NONE', ( #8779, #2161, #7367 ) ) ;
#8393 = CARTESIAN_POINT ( 'NONE',  ( -1.071796769724496334, -20.49920871091334362, -11.96821117534496892 ) ) ;
#8394 = CARTESIAN_POINT ( 'NONE',  ( 4.000000000000003553, -20.45448218005117624, -8.956865794039782003 ) ) ;
#8395 = CARTESIAN_POINT ( 'NONE',  ( 3.500000000000000444, 36.74680007765648071, -0.05647727720536935281 ) ) ;
#8396 = EDGE_CURVE ( 'NONE', #5051, #14905, #662, .T. ) ;
#8397 = PRODUCT_DEFINITION_CONTEXT ( 'detailed design', #630, 'design' ) ;
#8398 = ORIENTED_EDGE ( 'NONE', *, *, #7387, .T. ) ;
#8399 = CARTESIAN_POINT ( 'NONE',  ( -4.000000000000004441, -24.10892870809205135, -6.123320504649964136 ) ) ;
#8400 = FILL_AREA_STYLE_COLOUR ( '', #8335 ) ;
#8401 = CARTESIAN_POINT ( 'NONE',  ( -2.829195390882805139, 18.37180007765647360, -3.793023760679206102 ) ) ;
#8402 = UNCERTAINTY_MEASURE_WITH_UNIT (LENGTH_MEASURE( 1.000000000000000082E-05 ), #15835, 'distance_accuracy_value', 'NONE');
#8403 = LINE ( 'NONE', #12397, #8966 ) ;
#8404 = CARTESIAN_POINT ( 'NONE',  ( 2.518350579753611207, 35.62819992234354771, -0.7558219633769606149 ) ) ;
#8405 = ORIENTED_EDGE ( 'NONE', *, *, #11348, .T. ) ;
#8406 = CARTESIAN_POINT ( 'NONE',  ( 2.121784821874994176, -27.85708337327849549, -9.095322858313648950 ) ) ;
#8407 = EDGE_CURVE ( 'NONE', #5921, #15102, #6278, .T. ) ;
#8408 = CARTESIAN_POINT ( 'NONE',  ( 3.673772985318219053, 36.99680007765647360, 2.599342558260951730 ) ) ;
#8409 = ORIENTED_EDGE ( 'NONE', *, *, #1512, .F. ) ;
#8410 = SURFACE_STYLE_FILL_AREA ( #17144 ) ;
#8411 = CARTESIAN_POINT ( 'NONE',  ( -8.000000000000000000, 13.00000000000000178, 2.500000000000000000 ) ) ;
#8412 = DIRECTION ( 'NONE',  ( 0.000000000000000000, 1.000000000000000000, 0.000000000000000000 ) ) ;
#8413 = CARTESIAN_POINT ( 'NONE',  ( -4.243569643750005227, -25.36948240980282421, -7.678405556576772817 ) ) ;
#8414 = ORIENTED_EDGE ( 'NONE', *, *, #2173, .T. ) ;
#8415 = DIRECTION ( 'NONE',  ( -4.915049848600951133E-16, 0.000000000000000000, -1.000000000000000000 ) ) ;
#8416 = EDGE_CURVE ( 'NONE', #5122, #5664, #12783, .T. ) ;
#8417 = EDGE_LOOP ( 'NONE', ( #1597, #6748 ) ) ;
#8418 = CARTESIAN_POINT ( 'NONE',  ( 4.000000000000003553, -23.03557614363086259, -12.64304999334026114 ) ) ;
#8419 = DIRECTION ( 'NONE',  ( 0.000000000000000000, -1.000000000000000000, 0.000000000000000000 ) ) ;
#8420 = LINE ( 'NONE', #10076, #11035 ) ;
#8421 =( NAMED_UNIT ( * ) PLANE_ANGLE_UNIT ( ) SI_UNIT ( $, .RADIAN. ) );
#8422 = CARTESIAN_POINT ( 'NONE',  ( 4.481649420246397675, 20.87819992234354416, 1.518615910253363177 ) ) ;
#8423 = CARTESIAN_POINT ( 'NONE',  ( 1.135272562821020070, 22.75319992234354416, -3.311245368580577164 ) ) ;
#8424 = CARTESIAN_POINT ( 'NONE',  ( -4.000000000000004441, -28.49678844617752205, -12.38983364346077565 ) ) ;
#8425 = CARTESIAN_POINT ( 'NONE',  ( 0.8262555684461332373, 37.24680007765648071, 2.360188852285403982 ) ) ;
#8426 = CARTESIAN_POINT ( 'NONE',  ( -4.518350579753602325, 36.87819992234354061, 1.405661355842794391 ) ) ;
#8427 = CARTESIAN_POINT ( 'NONE',  ( 4.000000000000000888, -23.85187093787765278, -9.782521869579230867 ) ) ;
#8428 = ORIENTED_EDGE ( 'NONE', *, *, #131, .T. ) ;
#8429 = CARTESIAN_POINT ( 'NONE',  ( 3.999999999999996447, -22.73234526084956286, -4.157355598356369697 ) ) ;
#8430 = CARTESIAN_POINT ( 'NONE',  ( -2.211161402132902243, 18.37180007765647005, -2.942372952327172886 ) ) ;
#8431 = CARTESIAN_POINT ( 'NONE',  ( -5.330712181944246111E-15, -27.55925376772441382, -6.534233044972094895 ) ) ;
#8432 = ADVANCED_FACE ( 'NONE', ( #11214 ), #1863, .F. ) ;
#8433 = CARTESIAN_POINT ( 'NONE',  ( 3.673772985318219053, 21.99680007765647716, 2.599342558260951730 ) ) ;
#8434 = CARTESIAN_POINT ( 'NONE',  ( 2.343145750507615865, 4.000000000000006217, -3.999999999999999112 ) ) ;
#8435 = DIRECTION ( 'NONE',  ( -0.000000000000000000, 1.000000000000000000, -0.000000000000000000 ) ) ;
#8436 = ORIENTED_EDGE ( 'NONE', *, *, #16928, .T. ) ;
#8437 = EDGE_LOOP ( 'NONE', ( #7685, #15667, #7578, #12011 ) ) ;
#8438 = CARTESIAN_POINT ( 'NONE',  ( 2.864755990943265829, 26.99680007765648071, 2.011557305968487697 ) ) ;
#8439 = CYLINDRICAL_SURFACE ( 'NONE', #7564, 0.9999999999999991118 ) ;
#8440 = CARTESIAN_POINT ( 'NONE',  ( 2.000000000000004441, -18.19655077534320498, -7.745364512584909988 ) ) ;
#8441 = ORIENTED_EDGE ( 'NONE', *, *, #13744, .F. ) ;
#8442 = CARTESIAN_POINT ( 'NONE',  ( 3.518350579753605434, 20.62819992234354771, -1.080741659609877114 ) ) ;
#8443 = CARTESIAN_POINT ( 'NONE',  ( -2.121784821875005722, -26.31918155331226217, -6.898971439563784003 ) ) ;
#8444 = CARTESIAN_POINT ( 'NONE',  ( -3.481649420246369697, 35.37180007765648071, 1.193696214020542490 ) ) ;
#8445 = CARTESIAN_POINT ( 'NONE',  ( 2.798362969681409851, 28.50319992234354416, 2.102939460078764977 ) ) ;
#8446 = CARTESIAN_POINT ( 'NONE',  ( -2.000000000000005773, -24.00085731285198065, -3.955819603412733976 ) ) ;
#8447 = CARTESIAN_POINT ( 'NONE',  ( -12.99999999999999822, 15.00000000000000000, -16.00000000000000000 ) ) ;
#8448 = CARTESIAN_POINT ( 'NONE',  ( -4.243569643750000786, -24.67459463912114259, -10.95749308360964136 ) ) ;
#8449 = AXIS2_PLACEMENT_3D ( 'NONE', #1843, #14735, #2034 ) ;
#8450 = ADVANCED_FACE ( 'NONE', ( #15236 ), #1358, .F. ) ;
#8451 = DIRECTION ( 'NONE',  ( 0.000000000000000000, 0.000000000000000000, 1.000000000000000000 ) ) ;
#8452 = DIRECTION ( 'NONE',  ( -0.000000000000000000, 1.000000000000000000, -0.000000000000000000 ) ) ;
#8453 = CARTESIAN_POINT ( 'NONE',  ( -5.330712181944245322E-15, -23.94572221871285578, -1.373575165951426369 ) ) ;
#8454 = TOROIDAL_SURFACE ( 'NONE', #490, 9.000000000000001776, 0.9999999999999991118 ) ;
#8455 = EDGE_CURVE ( 'NONE', #8864, #4535, #4771, .T. ) ;
#8456 = DIRECTION ( 'NONE',  ( 0.000000000000000000, 0.000000000000000000, 1.000000000000000000 ) ) ;
#8457 = ORIENTED_EDGE ( 'NONE', *, *, #14795, .F. ) ;
#8458 = CARTESIAN_POINT ( 'NONE',  ( -1.593127413382952939, 19.12819992234354771, 2.091722143975172532 ) ) ;
#8459 = ADVANCED_FACE ( 'NONE', ( #5834 ), #15678, .T. ) ;
#8460 = CIRCLE ( 'NONE', #12909, 0.9999999999999991118 ) ;
#8461 = CARTESIAN_POINT ( 'NONE',  ( 2.121784821875004390, -23.78282679764076590, -16.09115178578480254 ) ) ;
#8462 = CARTESIAN_POINT ( 'NONE',  ( 2.115076519116362963, 38.87180007765645939, -3.012182706137107591 ) ) ;
#8463 = DIRECTION ( 'NONE',  ( 0.000000000000000000, 0.000000000000000000, -1.000000000000000000 ) ) ;
#8464 = ORIENTED_EDGE ( 'NONE', *, *, #15238, .T. ) ;
#8465 = CARTESIAN_POINT ( 'NONE',  ( 2.769796806539087886, -22.38185710306395393, -1.928164938508226456 ) ) ;
#8466 = CARTESIAN_POINT ( 'NONE',  ( -2.864755990943265829, 30.74680007765647716, -2.011557305968488141 ) ) ;
#8467 = DIRECTION ( 'NONE',  ( 0.000000000000000000, 0.000000000000000000, 1.000000000000000000 ) ) ;
#8468 = AXIS2_PLACEMENT_3D ( 'NONE', #18050, #11147, #9580 ) ;
#8469 = CARTESIAN_POINT ( 'NONE',  ( -4.243569643749998122, -24.20555259025267958, -14.55912172808130478 ) ) ;
#8470 = CARTESIAN_POINT ( 'NONE',  ( 9.000000000000005329, 18.79999999999999361, 2.499999999999997335 ) ) ;
#8471 = DIRECTION ( 'NONE',  ( -0.000000000000000000, -0.000000000000000000, -1.000000000000000000 ) ) ;
#8472 = DIRECTION ( 'NONE',  ( 0.000000000000000000, 1.000000000000000000, 0.000000000000000000 ) ) ;
#8473 = CARTESIAN_POINT ( 'NONE',  ( -4.243569643749997233, -22.14067741938892908, -11.61017436864092112 ) ) ;
#8474 = ORIENTED_EDGE ( 'NONE', *, *, #9762, .F. ) ;
#8475 = CARTESIAN_POINT ( 'NONE',  ( -1.999999999999996225, -20.92820855276008629, -11.64657612250448437 ) ) ;
#8476 = CARTESIAN_POINT ( 'NONE',  ( 3.999999999999996447, -21.95801707177565731, -3.051500338566227821 ) ) ;
#8477 = CARTESIAN_POINT ( 'NONE',  ( -2.115076519116362519, 40.12180007765648071, 3.012182706137107147 ) ) ;
#8478 = EDGE_LOOP ( 'NONE', ( #6283, #14604, #16192, #16324 ) ) ;
#8479 =( BOUNDED_CURVE ( )  B_SPLINE_CURVE ( 2, ( #3323, #10164, #11935, #358, #7481, #15840, #449, #17345, #7572 ),
 .UNSPECIFIED., .F., .F. ) 
 B_SPLINE_CURVE_WITH_KNOTS ( ( 3, 2, 2, 2, 3 ),
 ( 0.6120689655172414367, 0.6149425287356321546, 0.6206896551724138122, 0.6264367816091953589, 0.6293103448275861878 ),
 .UNSPECIFIED. ) 
 CURVE ( )  GEOMETRIC_REPRESENTATION_ITEM ( )  RATIONAL_B_SPLINE_CURVE ( ( 0.9330127018922194093, 0.9330127018922206306, 1.000000000000000000, 0.8660254037844387076, 1.000000000000000000, 0.8660254037844387076, 1.000000000000000000, 0.9330127018922194093, 0.9330127018922194093 ) ) 
 REPRESENTATION_ITEM ( '' )  );
#8480 = DIRECTION ( 'NONE',  ( -0.000000000000000000, -0.5735764363510414965, -0.8191520442889950182 ) ) ;
#8481 = SURFACE_SIDE_STYLE ('',( #15641 ) ) ;
#8482 = CARTESIAN_POINT ( 'NONE',  ( 0.3999999999999975797, 7.960204194457795477E-16, -6.500000000000000000 ) ) ;
#8483 = AXIS2_PLACEMENT_3D ( 'NONE', #13829, #14353, #1138 ) ;
#8484 = CARTESIAN_POINT ( 'NONE',  ( -1.989345975306457071, 32.25319992234354061, -1.515154207786300944 ) ) ;
#8485 = VERTEX_POINT ( 'NONE', #14373 ) ;
#8486 = CARTESIAN_POINT ( 'NONE',  ( 4.243569643749997233, -26.83210232249799532, -9.767243269513704362 ) ) ;
#8487 = CARTESIAN_POINT ( 'NONE',  ( 4.518350579753633411, 36.87180007765647360, 1.405661355842698468 ) ) ;
#8488 = ORIENTED_EDGE ( 'NONE', *, *, #12813, .F. ) ;
#8489 = CARTESIAN_POINT ( 'NONE',  ( 0.000000000000000000, -1.759474945355381292, 3.047500000000002540 ) ) ;
#8490 = CARTESIAN_POINT ( 'NONE',  ( -5.577813053751546416E-15, -28.99977223862889275, -10.16069966866791141 ) ) ;
#8491 = EDGE_CURVE ( 'NONE', #18179, #18256, #16534, .T. ) ;
#8492 = LINE ( 'NONE', #7381, #6085 ) ;
#8493 = AXIS2_PLACEMENT_3D ( 'NONE', #168, #454, #3238 ) ;
#8494 = DIRECTION ( 'NONE',  ( 0.000000000000000000, 0.000000000000000000, 1.000000000000000000 ) ) ;
#8496 = CARTESIAN_POINT ( 'NONE',  ( 9.000000000000001776, 27.59999999999999432, -2.500000000000002665 ) ) ;
#8495 = AXIS2_PLACEMENT_3D ( 'NONE', #14239, #12469, #9871 ) ;
#8497 = CARTESIAN_POINT ( 'NONE',  ( -4.243569643750000786, -22.35161007189942595, -7.639927304239214401 ) ) ;
#8498 = ORIENTED_EDGE ( 'NONE', *, *, #7500, .F. ) ;
#8499 = DIRECTION ( 'NONE',  ( 0.000000000000000000, 0.8191520442889952403, -0.5735764363510413855 ) ) ;
#8500 = ORIENTED_EDGE ( 'NONE', *, *, #18026, .T. ) ;
#8501 = CARTESIAN_POINT ( 'NONE',  ( -1.999999999999996225, -22.28328288434436644, -13.58182282814399855 ) ) ;
#8502 = CARTESIAN_POINT ( 'NONE',  ( 4.299564228933482956E-15, -17.21984060877302269, -7.284788156899542066 ) ) ;
#8503 = CARTESIAN_POINT ( 'NONE',  ( 2.399999999999999911, 0.000000000000000000, 2.000000000000000000 ) ) ;
#8504 = CARTESIAN_POINT ( 'NONE',  ( 1.444289557195957086, 15.25319992234354594, -4.262301884875733471 ) ) ;
#8505 = CARTESIAN_POINT ( 'NONE',  ( 1.027846397803612311, 28.75319992234354416, 3.346150245485499219 ) ) ;
#8506 = CARTESIAN_POINT ( 'NONE',  ( 4.000000000000000888, -25.98127345853583847, -12.82362383500889003 ) ) ;
#8507 = CARTESIAN_POINT ( 'NONE',  ( -1.989345975306457071, 14.75319992234354771, -1.515154207786300944 ) ) ;
#8508 = AXIS2_PLACEMENT_3D ( 'NONE', #1905, #502, #3096 ) ;
#8509 = CARTESIAN_POINT ( 'NONE',  ( -3.607379964056363075, 34.75319992234354771, -2.690724712371229899 ) ) ;
#8510 = CIRCLE ( 'NONE', #12357, 0.9999999999999991118 ) ;
#8511 = CARTESIAN_POINT ( 'NONE',  ( 4.713407268011036227E-15, -20.00384236256828885, -12.33960334402152270 ) ) ;
#8512 = VERTEX_POINT ( 'NONE', #3703 ) ;
#8513 = EDGE_CURVE ( 'NONE', #1278, #3449, #9350, .T. ) ;
#8514 = CARTESIAN_POINT ( 'NONE',  ( 10.00000000000000355, 38.59999999999999432, 2.499999999999996891 ) ) ;
#8515 = EDGE_CURVE ( 'NONE', #17896, #5987, #10827, .T. ) ;
#8516 = CARTESIAN_POINT ( 'NONE',  ( -1.027846397803541700, 22.49680007765648071, 3.346150245485522312 ) ) ;
#8517 = CARTESIAN_POINT ( 'NONE',  ( -6.428571428571426161, -14.26578344203648463, -2.827263138854405611 ) ) ;
#8518 = CARTESIAN_POINT ( 'NONE',  ( -5.330712181944246111E-15, -26.52681618229254212, -5.059759365251904839 ) ) ;
#8519 = VECTOR ( 'NONE', #16291, 1000.000000000000000 ) ;
#8520 = CARTESIAN_POINT ( 'NONE',  ( -1.444289557196047014, 20.99680007765647360, -4.262301884875704161 ) ) ;
#8521 = CARTESIAN_POINT ( 'NONE',  ( -3.706921591972381904E-14, -16.70362181605707619, -6.547551317039444818 ) ) ;
#8522 = COLOUR_RGB ( '',0.8941176470588234615, 0.8941176470588234615, 0.8941176470588234615 ) ;
#8523 = CARTESIAN_POINT ( 'NONE',  ( 0.000000000000000000, 34.19999999999999574, 2.500000000000000000 ) ) ;
#8524 = ORIENTED_EDGE ( 'NONE', *, *, #3097, .F. ) ;
#8525 = AXIS2_PLACEMENT_3D ( 'NONE', #1900, #7530, #13183 ) ;
#8526 = ORIENTED_EDGE ( 'NONE', *, *, #7671, .T. ) ;
#8527 = CARTESIAN_POINT ( 'NONE',  ( 2.115076519116362963, 23.87180007765647005, -3.012182706137107147 ) ) ;
#8528 = CARTESIAN_POINT ( 'NONE',  ( 0.000000000000000000, 43.00000000000000000, 2.500000000000000000 ) ) ;
#8529 = SURFACE_STYLE_USAGE ( .BOTH. , #4278 ) ;
#8530 = DIRECTION ( 'NONE',  ( -0.000000000000000000, -1.000000000000000000, -0.000000000000000000 ) ) ;
#8531 = CARTESIAN_POINT ( 'NONE',  ( -4.000000000000004441, -28.75489784253548819, -12.75845206339082161 ) ) ;
#8532 = ORIENTED_EDGE ( 'NONE', *, *, #16511, .T. ) ;
#8533 = CARTESIAN_POINT ( 'NONE',  ( 2.798362969681409851, 18.50319992234354771, 2.102939460078764977 ) ) ;
#8534 = CARTESIAN_POINT ( 'NONE',  ( 2.121784821875004390, -19.65307645591326846, -10.19325706690404054 ) ) ;
#8535 = CARTESIAN_POINT ( 'NONE',  ( 2.864755990943265829, 39.49680007765647360, 2.011557305968487697 ) ) ;
#8536 = CARTESIAN_POINT ( 'NONE',  ( 1.027846397803612311, 33.75319992234354771, 3.346150245485499219 ) ) ;
#8537 = PLANE ( 'NONE',  #11997 ) ;
#8538 = CARTESIAN_POINT ( 'NONE',  ( 4.000000000000000888, -27.20729309053124112, -14.57456132866984966 ) ) ;
#8539 = AXIS2_PLACEMENT_3D ( 'NONE', #4224, #9781, #5249 ) ;
#8540 = CARTESIAN_POINT ( 'NONE',  ( 2.121784821874994176, -25.01788001334084299, -5.040520239083123855 ) ) ;
#8541 = CARTESIAN_POINT ( 'NONE',  ( 2.000000000000004441, -24.13306689157648321, -16.22358817097600436 ) ) ;
#8542 = EDGE_CURVE ( 'NONE', #11668, #10052, #12559, .T. ) ;
#8543 = DIRECTION ( 'NONE',  ( 0.000000000000000000, 0.000000000000000000, 1.000000000000000000 ) ) ;
#8544 = CARTESIAN_POINT ( 'NONE',  ( -8.500000000000010658, 15.00000000000000178, 20.49999999999998934 ) ) ;
#8545 = CARTESIAN_POINT ( 'NONE',  ( -4.243569643749997233, -19.04336466309330689, -7.186753329480350061 ) ) ;
#8546 = CARTESIAN_POINT ( 'NONE',  ( -2.900082530493758526, 15.00000000000002309, -0.8289172060808163156 ) ) ;
#8547 =( NAMED_UNIT ( * ) SI_UNIT ( $, .STERADIAN. ) SOLID_ANGLE_UNIT ( ) );
#8548 = ORIENTED_EDGE ( 'NONE', *, *, #7503, .T. ) ;
#8549 = CIRCLE ( 'NONE', #13303, 10.00000000000000000 ) ;
#8550 = CARTESIAN_POINT ( 'NONE',  ( 2.518350579753611207, 18.12819992234354416, -0.7558219633769606149 ) ) ;
#8551 = FACE_OUTER_BOUND ( 'NONE', #2673, .T. ) ;
#8552 = CARTESIAN_POINT ( 'NONE',  ( -0.05938372350927861171, 18.62180007765647005, -3.680117784833935701 ) ) ;
#8553 = CARTESIAN_POINT ( 'NONE',  ( 9.999999999999998224, 25.39999999999999503, -2.500000000000001776 ) ) ;
#8554 = CARTESIAN_POINT ( 'NONE',  ( -13.00000000000000178, 13.00000000000000178, -25.00000000000000355 ) ) ;
#8555 = EDGE_LOOP ( 'NONE', ( #2049, #5241, #11223, #16936 ) ) ;
#8556 = CARTESIAN_POINT ( 'NONE',  ( -4.243569643749998122, -18.55940954492211503, -6.495593792111509224 ) ) ;
#8557 = CARTESIAN_POINT ( 'NONE',  ( -2.798362969681365886, 35.24680007765648071, 2.102939460078824929 ) ) ;
#8558 = AXIS2_PLACEMENT_3D ( 'NONE', #12821, #5600, #4208 ) ;
#8559 = ADVANCED_FACE ( 'NONE', ( #10656 ), #17326, .T. ) ;
#8560 = PRESENTATION_LAYER_ASSIGNMENT (  '', '', ( #5411 ) ) ;
#8561 = AXIS2_PLACEMENT_3D ( 'NONE', #6439, #16284, #13393 ) ;
#8562 = DIRECTION ( 'NONE',  ( 0.000000000000000000, 0.000000000000000000, -1.000000000000000000 ) ) ;
#8563 = CARTESIAN_POINT ( 'NONE',  ( 4.730628863548789710E-15, -21.20918936871244398, -14.55136167740457864 ) ) ;
#8564 = CARTESIAN_POINT ( 'NONE',  ( -1.734723475976807094E-15, 20.99999999999999289, -2.500000000000000000 ) ) ;
#8565 = ADVANCED_FACE ( 'NONE', ( #13524 ), #7502, .F. ) ;
#8566 = CARTESIAN_POINT ( 'NONE',  ( 8.499999999999992895, 14.99364916731036956, 20.49999999999999645 ) ) ;
#8567 = CARTESIAN_POINT ( 'NONE',  ( -1.734723475976807094E-15, 40.79999999999999716, -2.500000000000000000 ) ) ;
#8568 = CARTESIAN_POINT ( 'NONE',  ( -4.243569643750000786, -24.12611217186045565, -10.17417894125829037 ) ) ;
#8569 = CARTESIAN_POINT ( 'NONE',  ( 2.000000000000004441, -18.97087896441710697, -8.851219772375051420 ) ) ;
#8570 = CARTESIAN_POINT ( 'NONE',  ( 2.000000000000004441, -16.90600379355336003, -5.902272412934671308 ) ) ;
#8571 = CARTESIAN_POINT ( 'NONE',  ( -2.055738996568313048, 23.24680007765648071, -1.423772053676023441 ) ) ;
#8572 = ORIENTED_EDGE ( 'NONE', *, *, #14532, .F. ) ;
#8573 = CARTESIAN_POINT ( 'NONE',  ( -2.211161402132901799, 20.87180007765647360, -2.942372952327172886 ) ) ;
#8574 = CARTESIAN_POINT ( 'NONE',  ( -9.000000000000003553, 34.19999999999999574, -2.500000000000001776 ) ) ;
#8575 =( NAMED_UNIT ( * ) PLANE_ANGLE_UNIT ( ) SI_UNIT ( $, .RADIAN. ) );
#8576 = CIRCLE ( 'NONE', #7404, 0.9999999999999991118 ) ;
#8577 = CARTESIAN_POINT ( 'NONE',  ( -1.071796769724496334, -26.23662292920451478, -6.214513490082579139 ) ) ;
#8578 = CARTESIAN_POINT ( 'NONE',  ( -3.481649420246394122, 14.62819992234354061, -1.193696214020467883 ) ) ;
#8579 = ORIENTED_EDGE ( 'NONE', *, *, #5682, .T. ) ;
#8580 = CARTESIAN_POINT ( 'NONE',  ( 4.243569643749997233, -25.79966473706611652, -8.292769589793515195 ) ) ;
#8581 = CARTESIAN_POINT ( 'NONE',  ( 2.829195390882805583, 29.62180007765647005, 3.793023760679204770 ) ) ;
#8582 = VERTEX_POINT ( 'NONE', #16328 ) ;
#8583 = EDGE_CURVE ( 'NONE', #13628, #16136, #4726, .T. ) ;
#8584 = CARTESIAN_POINT ( 'NONE',  ( -2.000000000000005773, -25.29140429464182560, -5.798911703062972656 ) ) ;
#8585 = CARTESIAN_POINT ( 'NONE',  ( 15.00000000000000355, -10.00000000000000000, 30.00000000000000000 ) ) ;
#8586 = AXIS2_PLACEMENT_3D ( 'NONE', #18169, #11353, #12658 ) ;
#8587 = CARTESIAN_POINT ( 'NONE',  ( -6.158835246850665095E-15, -22.64013793229036864, -15.02577497543054186 ) ) ;
#8588 = CARTESIAN_POINT ( 'NONE',  ( -5.577813053751546416E-15, -29.51599103134483570, -10.89793650852800511 ) ) ;
#8589 =( BOUNDED_CURVE ( )  B_SPLINE_CURVE ( 2, ( #12063, #687, #773, #4933, #6236, #11789, #10587 ),
 .UNSPECIFIED., .F., .F. ) 
 B_SPLINE_CURVE_WITH_KNOTS ( ( 3, 2, 2, 3 ),
 ( 0.03070921116881014309, 0.03448275862068965469, 0.04022988505747126381, 0.04310344827586207184 ),
 .UNSPECIFIED. ) 
 CURVE ( )  GEOMETRIC_REPRESENTATION_ITEM ( )  RATIONAL_B_SPLINE_CURVE ( ( 0.9395835397632845698, 0.9120326476671477556, 1.000000000000000000, 0.8660254037844387076, 1.000000000000000000, 0.9330127018922192983, 0.9330127018922194093 ) ) 
 REPRESENTATION_ITEM ( '' )  );
#8590 = CARTESIAN_POINT ( 'NONE',  ( 4.243569643750003451, -18.90355540673274248, -6.987085018684902948 ) ) ;
#8591 = EDGE_LOOP ( 'NONE', ( #7162, #4503, #4656, #3071, #5827, #7231 ) ) ;
#8592 = CARTESIAN_POINT ( 'NONE',  ( 1.071796769724485232, -26.40715157433038129, -6.458053634711515834 ) ) ;
#8593 = ORIENTED_EDGE ( 'NONE', *, *, #2463, .T. ) ;
#8594 = VERTEX_POINT ( 'NONE', #14668 ) ;
#8595 = CARTESIAN_POINT ( 'NONE',  ( -1.734723475976807094E-15, 25.39999999999999503, -2.500000000000000000 ) ) ;
#8596 = CARTESIAN_POINT ( 'NONE',  ( 3.607379964056363075, 21.00319992234354416, 2.690724712371229010 ) ) ;
#8597 = CARTESIAN_POINT ( 'NONE',  ( -0.05938372350920064630, 26.37819992234354416, 3.680117784833935701 ) ) ;
#8598 = CARTESIAN_POINT ( 'NONE',  ( 2.055738996568313048, 34.49680007765648071, 1.423772053676023441 ) ) ;
#8599 = ORIENTED_EDGE ( 'NONE', *, *, #4973, .T. ) ;
#8600 = CARTESIAN_POINT ( 'NONE',  ( 2.733110507866328920, 33.62819992234354771, 3.862833514489095510 ) ) ;
#8601 = CARTESIAN_POINT ( 'NONE',  ( -3.999999999999997335, -21.59446534659391759, -10.58493048105740009 ) ) ;
#8602 = VERTEX_POINT ( 'NONE', #2148 ) ;
#8603 = DIRECTION ( 'NONE',  ( -3.373073425510457965E-16, 0.000000000000000000, -1.000000000000000000 ) ) ;
#8604 = CARTESIAN_POINT ( 'NONE',  ( -0.05938372350927861171, 28.62180007765648071, -3.680117784833935701 ) ) ;
#8605 = CARTESIAN_POINT ( 'NONE',  ( -7.634097544908422073, -10.16870601894835069, 11.61220938195502583 ) ) ;
#8606 = CARTESIAN_POINT ( 'NONE',  ( -5.330712181944246111E-15, -26.78492557865051893, -5.428377785181952575 ) ) ;
#8607 = CARTESIAN_POINT ( 'NONE',  ( 2.829195390882805583, 34.62180007765646650, 3.793023760679204770 ) ) ;
#8608 = VECTOR ( 'NONE', #17384, 1000.000000000000000 ) ;
#8609 = DIRECTION ( 'NONE',  ( 1.000000000000000000, 0.000000000000000000, 0.000000000000000000 ) ) ;
#8610 = ORIENTED_EDGE ( 'NONE', *, *, #14908, .F. ) ;
#8611 = ORIENTED_EDGE ( 'NONE', *, *, #7508, .T. ) ;
#8612 = CARTESIAN_POINT ( 'NONE',  ( 2.211161402132902243, 27.12180007765647360, 2.942372952327172442 ) ) ;
#8613 = CARTESIAN_POINT ( 'NONE',  ( -6.903430137606132000, -10.00000000000000178, 15.77881270003272540 ) ) ;
#8614 = EDGE_CURVE ( 'NONE', #8360, #6360, #11860, .T. ) ;
#8615 =( LENGTH_UNIT ( ) NAMED_UNIT ( * ) SI_UNIT ( .MILLI., .METRE. ) );
#8616 = CARTESIAN_POINT ( 'NONE',  ( -13.00000000000000178, 15.00000000000000178, 25.00000000000000355 ) ) ;
#8617 = CARTESIAN_POINT ( 'NONE',  ( -1.661723472263481630E-14, -21.60770034685848984, -13.55130129571035447 ) ) ;
#8618 = ORIENTED_EDGE ( 'NONE', *, *, #7106, .T. ) ;
#8619 = CARTESIAN_POINT ( 'NONE',  ( -2.211161402132839182, 19.12819992234353705, 2.942372952327218627 ) ) ;
#8620 = EDGE_CURVE ( 'NONE', #17312, #2844, #7688, .T. ) ;
#8621 = CARTESIAN_POINT ( 'NONE',  ( -5.330712181944245322E-15, -26.26870678593457242, -4.691140945321855327 ) ) ;
#8622 = CARTESIAN_POINT ( 'NONE',  ( 3.518350579753631191, 36.87180007765645939, 1.080741659609802285 ) ) ;
#8623 = ADVANCED_FACE ( 'NONE', ( #4908 ), #12549, .F. ) ;
#8624 = CARTESIAN_POINT ( 'NONE',  ( 2.115076519116426024, 38.62819992234354771, 3.012182706137062294 ) ) ;
#8625 = DIRECTION ( 'NONE',  ( -1.000000000000000000, 0.000000000000000000, 0.000000000000000000 ) ) ;
#8626 = EDGE_CURVE ( 'NONE', #7494, #11376, #5129, .T. ) ;
#8627 = CARTESIAN_POINT ( 'NONE',  ( 4.243569643750000786, -22.99688356279435197, -8.561473354064329300 ) ) ;
#8628 = ADVANCED_FACE ( 'NONE', ( #1966 ), #6397, .F. ) ;
#8629 = CARTESIAN_POINT ( 'NONE',  ( 1.006530391514320222, -10.00000000000244782, -4.211315095031120670 ) ) ;
#8630 = CIRCLE ( 'NONE', #4217, 8.000000000000001776 ) ;
#8631 = CARTESIAN_POINT ( 'NONE',  ( 0.000000000000000000, -27.20729309053124112, -14.57456132866985321 ) ) ;
#8632 = AXIS2_PLACEMENT_3D ( 'NONE', #6029, #10192, #7790 ) ;
#8633 = CARTESIAN_POINT ( 'NONE',  ( 8.000000000000000000, 0.000000000000000000, 0.000000000000000000 ) ) ;
#8634 = CARTESIAN_POINT ( 'NONE',  ( -2.121784821875005722, -23.99619698609053842, -3.581405660193354379 ) ) ;
#8635 = PRODUCT_RELATED_PRODUCT_CATEGORY ( 'part', '', ( #4859 ) ) ;
#8636 = DIRECTION ( 'NONE',  ( -0.000000000000000000, 1.000000000000000000, -0.000000000000000000 ) ) ;
#8638 = CARTESIAN_POINT ( 'NONE',  ( 1.300000000000000044, -0.7216878364870317197, 1.250000000000000000 ) ) ;
#8637 =( GEOMETRIC_REPRESENTATION_CONTEXT ( 3 ) GLOBAL_UNCERTAINTY_ASSIGNED_CONTEXT ( ( #17974 ) ) GLOBAL_UNIT_ASSIGNED_CONTEXT ( ( #16959, #8575, #1370 ) ) REPRESENTATION_CONTEXT ( 'NONE', 'WORKASPACE' ) );
#8639 = VERTEX_POINT ( 'NONE', #10472 ) ;
#8640 = CARTESIAN_POINT ( 'NONE',  ( -2.481649420246391902, 19.62819992234354416, -0.8687765177875723666 ) ) ;
#8641 = CARTESIAN_POINT ( 'NONE',  ( -5.330712181944245322E-15, -30.91467592037801282, -11.32627250406271635 ) ) ;
#8642 = DIRECTION ( 'NONE',  ( -1.000000000000000000, 0.000000000000000000, 0.000000000000000000 ) ) ;
#8643 = DIRECTION ( 'NONE',  ( 0.000000000000000000, 0.000000000000000000, -1.000000000000000000 ) ) ;
#8644 = CARTESIAN_POINT ( 'NONE',  ( 4.551717183842062475, -10.00000000000000178, -2.180355508048892776 ) ) ;
#8645 = ORIENTED_EDGE ( 'NONE', *, *, #6159, .T. ) ;
#8646 = AXIS2_PLACEMENT_3D ( 'NONE', #10526, #625, #6363 ) ;
#8647 = CARTESIAN_POINT ( 'NONE',  ( 4.243569643750000786, -20.41578959921466918, -4.875289154763852828 ) ) ;
#8648 = CARTESIAN_POINT ( 'NONE',  ( -1.135272562821090014, 30.99680007765647716, -3.311245368580554072 ) ) ;
#8649 = AXIS2_PLACEMENT_3D ( 'NONE', #11131, #9741, #15422 ) ;
#8650 = CARTESIAN_POINT ( 'NONE',  ( 4.243569643750003451, -24.58196212660805458, -15.09669025714595314 ) ) ;
#8651 = CARTESIAN_POINT ( 'NONE',  ( -13.00000000000000178, 15.00000000000000178, -16.00000000000000000 ) ) ;
#8652 = CARTESIAN_POINT ( 'NONE',  ( 4.243569643750000786, -25.28760445547132107, -11.83296183094350340 ) ) ;
#8653 = DIRECTION ( 'NONE',  ( -0.000000000000000000, -1.000000000000000000, -0.000000000000000000 ) ) ;
#8654 = LINE ( 'NONE', #11261, #4062 ) ;
#8655 = CARTESIAN_POINT ( 'NONE',  ( -5.330712181944245322E-15, -29.10791014587222847, -8.745943564552380423 ) ) ;
#8656 = CARTESIAN_POINT ( 'NONE',  ( 1.071796769724485232, -25.18113194233497154, -4.707116141050555314 ) ) ;
#8657 = AXIS2_PLACEMENT_3D ( 'NONE', #17376, #16067, #11777 ) ;
#8658 = CARTESIAN_POINT ( 'NONE',  ( 2.000000000000004441, -17.93844137898523527, -7.376746092654861364 ) ) ;
#8659 =( GEOMETRIC_REPRESENTATION_CONTEXT ( 3 ) GLOBAL_UNCERTAINTY_ASSIGNED_CONTEXT ( ( #2682 ) ) GLOBAL_UNIT_ASSIGNED_CONTEXT ( ( #8615, #1595, #10480 ) ) REPRESENTATION_CONTEXT ( 'NONE', 'WORKASPACE' ) );
#8660 = CARTESIAN_POINT ( 'NONE',  ( 0.7188294034286049072, 18.74680007765648071, -2.395093729190366005 ) ) ;
#8661 = ORIENTED_EDGE ( 'NONE', *, *, #14627, .F. ) ;
#8662 = CARTESIAN_POINT ( 'NONE',  ( -3.518350579753630303, 25.62180007765647716, -1.080741659609802952 ) ) ;
#8663 = DIRECTION ( 'NONE',  ( -1.000000000000000000, 0.000000000000000000, 4.336808689942021680E-16 ) ) ;
#8664 = DIRECTION ( 'NONE',  ( 0.000000000000000000, -1.000000000000000000, 0.000000000000000000 ) ) ;
#8665 = CARTESIAN_POINT ( 'NONE',  ( 0.000000000000000000, 29.79999999999999716, 2.500000000000000000 ) ) ;
#8666 = CARTESIAN_POINT ( 'NONE',  ( 1.593127413382953383, 37.87819992234354771, -2.091722143975172532 ) ) ;
#8667 = ORIENTED_EDGE ( 'NONE', *, *, #2688, .T. ) ;
#8668 = CARTESIAN_POINT ( 'NONE',  ( -4.243569643749998122, -22.68915988664960892, -12.39348851099227389 ) ) ;
#8669 = CARTESIAN_POINT ( 'NONE',  ( -4.518350579753632523, 35.62180007765647360, -1.405661355842698468 ) ) ;
#8670 = VERTEX_POINT ( 'NONE', #7866 ) ;
#8671 = CIRCLE ( 'NONE', #16999, 8.000000000000003553 ) ;
#8672 = DIRECTION ( 'NONE',  ( -0.000000000000000000, -0.5735764363510414965, -0.8191520442889950182 ) ) ;
#8673 = DIRECTION ( 'NONE',  ( 0.000000000000000000, 0.000000000000000000, -1.000000000000000000 ) ) ;
#8674 = CARTESIAN_POINT ( 'NONE',  ( 0.000000000000000000, -0.7216878364870317197, -1.250000000000000000 ) ) ;
#8675 = DIRECTION ( 'NONE',  ( -0.000000000000000000, -1.000000000000000000, -0.000000000000000000 ) ) ;
#8676 = CARTESIAN_POINT ( 'NONE',  ( -1.071796769724486786, -17.40189595461771432, -7.544790136184399643 ) ) ;
#8677 = CARTESIAN_POINT ( 'NONE',  ( -4.243569643749997233, -18.81751894128008118, -6.864212212041558736 ) ) ;
#8678 = ORIENTED_EDGE ( 'NONE', *, *, #13789, .F. ) ;
#8679 = EDGE_CURVE ( 'NONE', #8864, #10774, #14448, .T. ) ;
#8680 = CARTESIAN_POINT ( 'NONE',  ( 0.000000000000000000, 5.977523610840987267, 32.81826849749789687 ) ) ;
#8681 = EDGE_LOOP ( 'NONE', ( #9439, #10411 ) ) ;
#8682 = VERTEX_POINT ( 'NONE', #12131 ) ;
#8683 = DIRECTION ( 'NONE',  ( -0.000000000000000000, -1.000000000000000000, -0.000000000000000000 ) ) ;
#8684 = AXIS2_PLACEMENT_3D ( 'NONE', #16277, #2002, #13295 ) ;
#8685 = FACE_OUTER_BOUND ( 'NONE', #4396, .T. ) ;
#8686 = SURFACE_SIDE_STYLE ('',( #7396 ) ) ;
#8687 = CARTESIAN_POINT ( 'NONE',  ( -2.733110507866328476, 19.87819992234354416, -3.862833514489096398 ) ) ;
#8688 = CARTESIAN_POINT ( 'NONE',  ( 3.518350579753606322, 25.62819992234354416, -1.080741659609876892 ) ) ;
#8689 = EDGE_CURVE ( 'NONE', #12954, #16136, #11501, .T. ) ;
#8690 = CARTESIAN_POINT ( 'NONE',  ( 0.8262555684460829442, 15.25319992234354771, -2.360188852285421302 ) ) ;
#8691 = EDGE_LOOP ( 'NONE', ( #2180, #6289, #11639, #14849 ) ) ;
#8692 = CARTESIAN_POINT ( 'NONE',  ( 3.607379964056363075, 36.00319992234354771, 2.690724712371229010 ) ) ;
#8693 = EDGE_CURVE ( 'NONE', #2518, #269, #15300, .T. ) ;
#8694 = CARTESIAN_POINT ( 'NONE',  ( -4.000000000000000888, -23.46470684334068935, -9.229594239684162815 ) ) ;
#8695 = VERTEX_POINT ( 'NONE', #4059 ) ;
#8696 = CARTESIAN_POINT ( 'NONE',  ( 3.999999999999996447, 6.938893903907228378E-15, 24.28148006742132026 ) ) ;
#8697 = CARTESIAN_POINT ( 'NONE',  ( 3.500000000000000444, 29.24680007765647716, -0.05647727720536935281 ) ) ;
#8698 =( BOUNDED_CURVE ( )  B_SPLINE_CURVE ( 2, ( #14027, #1429, #1337, #17195, #9756, #4467, #8446, #5854, #5677 ),
 .UNSPECIFIED., .F., .T. ) 
 B_SPLINE_CURVE_WITH_KNOTS ( ( 3, 2, 2, 2, 3 ),
 ( 0.7672413793103448620, 0.7701149425287355799, 0.7758620689655172376, 0.7816091954022988952, 0.7844827586206897241 ),
 .UNSPECIFIED. ) 
 CURVE ( )  GEOMETRIC_REPRESENTATION_ITEM ( )  RATIONAL_B_SPLINE_CURVE ( ( 0.9330127018922194093, 0.9330127018922206306, 1.000000000000000000, 0.8660254037844387076, 1.000000000000000000, 0.8660254037844387076, 1.000000000000000000, 0.9330127018922180770, 0.9330127018922194093 ) ) 
 REPRESENTATION_ITEM ( '' )  );
#8699 = DIRECTION ( 'NONE',  ( -3.469446951953613696E-16, -0.000000000000000000, -1.000000000000000000 ) ) ;
#8700 = CARTESIAN_POINT ( 'NONE',  ( 4.243569643750003451, -19.38751052490393789, -7.678244556053742897 ) ) ;
#8701 = CARTESIAN_POINT ( 'NONE',  ( -2.829195390882805139, 28.37180007765647716, -3.793023760679206102 ) ) ;
#8702 = DIRECTION ( 'NONE',  ( 0.000000000000000000, 0.000000000000000000, 1.000000000000000000 ) ) ;
#8703 = ORIENTED_EDGE ( 'NONE', *, *, #5649, .F. ) ;
#8704 = VERTEX_POINT ( 'NONE', #6929 ) ;
#8705 = CARTESIAN_POINT ( 'NONE',  ( 2.864755990943265829, 24.49680007765647716, 2.011557305968487697 ) ) ;
#8706 = EDGE_CURVE ( 'NONE', #11774, #646, #3990, .T. ) ;
#8707 = CARTESIAN_POINT ( 'NONE',  ( -15.00000000000000178, 10.00000000000000000, 24.99999999999999645 ) ) ;
#8708 = FACE_OUTER_BOUND ( 'NONE', #4245, .T. ) ;
#8709 = LINE ( 'NONE', #14201, #16072 ) ;
#8710 = SURFACE_STYLE_FILL_AREA ( #7230 ) ;
#8711 = EDGE_LOOP ( 'NONE', ( #15503, #8177 ) ) ;
#8712 = CARTESIAN_POINT ( 'NONE',  ( -2.211161402132839182, 16.62819992234354416, 2.942372952327218627 ) ) ;
#8713 = DIRECTION ( 'NONE',  ( 0.000000000000000000, 0.000000000000000000, 1.000000000000000000 ) ) ;
#8714 = CARTESIAN_POINT ( 'NONE',  ( -4.243569643750000786, -23.09367458642858040, -8.699705261538101198 ) ) ;
#8715 = CARTESIAN_POINT ( 'NONE',  ( 2.518350579753628971, 16.87180007765648071, 0.7558219633769073242 ) ) ;
#8716 = CARTESIAN_POINT ( 'NONE',  ( 3.518350579753605434, 35.62819992234353350, -1.080741659609877114 ) ) ;
#8717 = CARTESIAN_POINT ( 'NONE',  ( 7.960204194457794491E-16, 43.00000000000000000, 6.499999999999999112 ) ) ;
#8718 = COLOUR_RGB ( '',0.8941176470588234615, 0.8941176470588234615, 0.8941176470588234615 ) ;
#8719 = CARTESIAN_POINT ( 'NONE',  ( 2.199999999999999734, 2.694222958124177006E-16, -2.200000000000000178 ) ) ;
#8720 = CARTESIAN_POINT ( 'NONE',  ( 4.243569643750000786, -22.22255537372044998, -7.455618094274186092 ) ) ;
#8721 = CARTESIAN_POINT ( 'NONE',  ( -1.661723472263481630E-14, -20.51073541163217584, -11.98467301000088803 ) ) ;
#8722 = ADVANCED_FACE ( 'NONE', ( #1207 ), #14650, .T. ) ;
#8723 = CARTESIAN_POINT ( 'NONE',  ( -9.000000000000003553, 25.39999999999999503, -2.500000000000001776 ) ) ;
#8724 = DIRECTION ( 'NONE',  ( 1.000000000000000000, 0.000000000000000000, 0.000000000000000000 ) ) ;
#8725 = CARTESIAN_POINT ( 'NONE',  ( 14.20000000000000107, 1.971681346627238735E-16, -1.610000000000000098 ) ) ;
#8726 =( BOUNDED_CURVE ( )  B_SPLINE_CURVE ( 2, ( #8197, #16472, #5144, #12366, #8015, #16569, #1262, #2744, #5235 ),
 .UNSPECIFIED., .F., .F. ) 
 B_SPLINE_CURVE_WITH_KNOTS ( ( 3, 2, 2, 2, 3 ),
 ( 0.8879310344827586743, 0.8908045977011493921, 0.8965517241379310498, 0.9022988505747125965, 0.9051724137931034253 ),
 .UNSPECIFIED. ) 
 CURVE ( )  GEOMETRIC_REPRESENTATION_ITEM ( )  RATIONAL_B_SPLINE_CURVE ( ( 0.9330127018922194093, 0.9330127018922206306, 1.000000000000000000, 0.8660254037844387076, 1.000000000000000000, 0.8660254037844387076, 1.000000000000000000, 0.9330127018922194093, 0.9330127018922194093 ) ) 
 REPRESENTATION_ITEM ( '' )  );
#8727 = CARTESIAN_POINT ( 'NONE',  ( 2.121784821874994176, -23.17885056429031465, -2.414113997081532847 ) ) ;
#8728 = DIRECTION ( 'NONE',  ( 0.000000000000000000, 0.000000000000000000, -1.000000000000000000 ) ) ;
#8729 = DIRECTION ( 'NONE',  ( 0.000000000000000000, 0.000000000000000000, 1.000000000000000000 ) ) ;
#8730 = ORIENTED_EDGE ( 'NONE', *, *, #10501, .F. ) ;
#8731 = CARTESIAN_POINT ( 'NONE',  ( 2.055738996568281518, 20.50319992234355126, -1.423772053676066518 ) ) ;
#8732 = CARTESIAN_POINT ( 'NONE',  ( 4.730628863548789710E-15, -22.75784574686025152, -16.76307219698486506 ) ) ;
#8733 = CARTESIAN_POINT ( 'NONE',  ( -14.99999999999999645, 10.00000000000000000, -30.00000000000000000 ) ) ;
#8734 = CARTESIAN_POINT ( 'NONE',  ( -4.499999999999999112, 39.50319992234354061, -0.05647727720528529505 ) ) ;
#8735 = DIRECTION ( 'NONE',  ( -0.000000000000000000, -1.000000000000000000, -0.000000000000000000 ) ) ;
#8736 = CARTESIAN_POINT ( 'NONE',  ( 8.767957691173201340, -10.00000000000000178, -4.386791830708262729 ) ) ;
#8737 = ORIENTED_EDGE ( 'NONE', *, *, #7275, .T. ) ;
#8738 = CARTESIAN_POINT ( 'NONE',  ( -5.330712181944246111E-15, -24.23609528961556947, -1.788270888372731182 ) ) ;
#8739 = CARTESIAN_POINT ( 'NONE',  ( -3.481649420246369697, 37.87180007765648071, 1.193696214020542490 ) ) ;
#8740 = CARTESIAN_POINT ( 'NONE',  ( -4.243569643750000786, -26.73946980998488954, -13.90644044305002502 ) ) ;
#8741 = ADVANCED_FACE ( 'NONE', ( #15213 ), #9711, .T. ) ;
#8742 = EDGE_CURVE ( 'NONE', #12849, #16170, #17278, .T. ) ;
#8743 = DIRECTION ( 'NONE',  ( -3.469446951953613696E-16, -0.000000000000000000, -1.000000000000000000 ) ) ;
#8744 = EDGE_CURVE ( 'NONE', #3556, #11075, #6526, .T. ) ;
#8745 = CARTESIAN_POINT ( 'NONE',  ( 2.121784821874994176, -28.34103849144968379, -9.786482395682487123 ) ) ;
#8746 = AXIS2_PLACEMENT_3D ( 'NONE', #13743, #18306, #2809 ) ;
#8747 = CARTESIAN_POINT ( 'NONE',  ( -9.000000000000003553, 36.39999999999999147, -2.500000000000001776 ) ) ;
#8748 = CARTESIAN_POINT ( 'NONE',  ( 0.000000000000000000, 3.000000000000000000, 0.000000000000000000 ) ) ;
#8749 = CARTESIAN_POINT ( 'NONE',  ( 4.000000000000000888, -25.98127345853583847, -12.82362383500889003 ) ) ;
#8750 = AXIS2_PLACEMENT_3D ( 'NONE', #18367, #11279, #8769 ) ;
#8751 = CARTESIAN_POINT ( 'NONE',  ( -4.243569643750000786, -25.15854975729233090, -11.64865262097848309 ) ) ;
#8752 = DIRECTION ( 'NONE',  ( -0.000000000000000000, 1.000000000000000000, -0.000000000000000000 ) ) ;
#8753 = CARTESIAN_POINT ( 'NONE',  ( -4.000000000000004441, -22.30216293358627055, -3.542991565139629984 ) ) ;
#8754 = CARTESIAN_POINT ( 'NONE',  ( 1.593127413382998903, 19.62180007765648071, 2.091722143975139669 ) ) ;
#8755 = VERTEX_POINT ( 'NONE', #2693 ) ;
#8756 = CARTESIAN_POINT ( 'NONE',  ( -2.798362969681365886, 20.24680007765647716, 2.102939460078824929 ) ) ;
#8757 = CARTESIAN_POINT ( 'NONE',  ( 8.500000000000019540, 0.000000000000000000, -20.49999999999998934 ) ) ;
#8758 = DIRECTION ( 'NONE',  ( 0.000000000000000000, 0.000000000000000000, 1.000000000000000000 ) ) ;
#8759 = CIRCLE ( 'NONE', #790, 0.9999999999999991118 ) ;
#8760 = DIRECTION ( 'NONE',  ( 0.000000000000000000, 0.000000000000000000, -1.000000000000000000 ) ) ;
#8761 = CARTESIAN_POINT ( 'NONE',  ( -3.518350579753605434, 21.87819992234354771, 1.080741659609877781 ) ) ;
#8762 = ORIENTED_EDGE ( 'NONE', *, *, #3041, .F. ) ;
#8763 = CARTESIAN_POINT ( 'NONE',  ( -5.330712181944246111E-15, -27.59151744226916492, -6.580310347463351306 ) ) ;
#8764 = CARTESIAN_POINT ( 'NONE',  ( -1.336863392178478716, 34.99680007765647360, 4.297206761780677731 ) ) ;
#8765 = AXIS2_PLACEMENT_3D ( 'NONE', #3020, #8653, #17509 ) ;
#8766 = EDGE_LOOP ( 'NONE', ( #12252, #8159, #17455, #2499, #17236 ) ) ;
#8767 = CARTESIAN_POINT ( 'NONE',  ( -3.706921591972381904E-14, -16.70362181605707619, -6.547551317039444818 ) ) ;
#8768 = CARTESIAN_POINT ( 'NONE',  ( -4.243569643749997233, -23.20537867936554832, -13.13072535085237114 ) ) ;
#8769 = DIRECTION ( 'NONE',  ( 0.000000000000000000, 0.000000000000000000, 1.000000000000000000 ) ) ;
#8770 = DIRECTION ( 'NONE',  ( 0.000000000000000000, 0.000000000000000000, 1.000000000000000000 ) ) ;
#8771 = CARTESIAN_POINT ( 'NONE',  ( 4.000000000000003553, -21.74502916184101409, -10.79995789369002246 ) ) ;
#8772 = CARTESIAN_POINT ( 'NONE',  ( -2.121784821874996396, -18.35177491594184218, -8.334805866423387499 ) ) ;
#8773 = VERTEX_POINT ( 'NONE', #11193 ) ;
#8774 = EDGE_CURVE ( 'NONE', #2342, #12052, #953, .T. ) ;
#8775 = CARTESIAN_POINT ( 'NONE',  ( 1.071796769724485232, -24.34227640346663080, -3.509106275271134834 ) ) ;
#8776 = CARTESIAN_POINT ( 'NONE',  ( -10.00000000000000000, 31.99999999999999289, 2.499999999999996003 ) ) ;
#8777 = ORIENTED_EDGE ( 'NONE', *, *, #10734, .T. ) ;
#8778 = AXIS2_PLACEMENT_3D ( 'NONE', #10698, #12267, #16374 ) ;
#8779 = ORIENTED_EDGE ( 'NONE', *, *, #4223, .F. ) ;
#8780 = DIRECTION ( 'NONE',  ( -0.000000000000000000, -1.000000000000000000, -0.000000000000000000 ) ) ;
#8781 = DIRECTION ( 'NONE',  ( 0.000000000000000000, 0.000000000000000000, -1.000000000000000000 ) ) ;
#8782 = CARTESIAN_POINT ( 'NONE',  ( 3.607379964056363075, 23.50319992234354416, 2.690724712371229010 ) ) ;
#8783 = CARTESIAN_POINT ( 'NONE',  ( 2.864755990943222308, 30.50319992234354416, -2.011557305968548093 ) ) ;
#8784 = CARTESIAN_POINT ( 'NONE',  ( 2.481649420246374138, 36.62180007765647360, -0.8687765177876252132 ) ) ;
#8785 = ORIENTED_EDGE ( 'NONE', *, *, #17114, .T. ) ;
#8786 = CARTESIAN_POINT ( 'NONE',  ( 3.673772985318163098, 33.00319992234354771, -2.599342558261029001 ) ) ;
#8787 = EDGE_CURVE ( 'NONE', #9317, #4535, #18098, .T. ) ;
#8788 = CARTESIAN_POINT ( 'NONE',  ( 4.000000000000000888, -21.52888637065593258, -6.464956090208799466 ) ) ;
#8789 = ORIENTED_EDGE ( 'NONE', *, *, #7710, .T. ) ;
#8790 = CIRCLE ( 'NONE', #822, 2.149999999999999023 ) ;
#8791 = CARTESIAN_POINT ( 'NONE',  ( 9.000000000000000000, 43.00000000000000000, -2.500000000000001332 ) ) ;
#8792 = VECTOR ( 'NONE', #15746, 1000.000000000000000 ) ;
#8793 = CARTESIAN_POINT ( 'NONE',  ( 0.05938372350927906274, 27.37180007765647716, 3.680117784833935701 ) ) ;
#8794 = EDGE_CURVE ( 'NONE', #15303, #5033, #2331, .T. ) ;
#8795 = CARTESIAN_POINT ( 'NONE',  ( -9.930521455883233983, -9.929686425557429530, 8.932771133217334736 ) ) ;
#8796 = CARTESIAN_POINT ( 'NONE',  ( -2.121784821874996396, -18.06140184503912494, -7.920110144002082464 ) ) ;
#8797 = EDGE_CURVE ( 'NONE', #8602, #6560, #7263, .T. ) ;
#8798 = CARTESIAN_POINT ( 'NONE',  ( -1.444289557196047014, 30.99680007765647716, -4.262301884875704161 ) ) ;
#8799 = DIRECTION ( 'NONE',  ( -1.000000000000000000, 0.000000000000000000, 0.000000000000000000 ) ) ;
#8800 = EDGE_LOOP ( 'NONE', ( #17884, #3286, #596 ) ) ;
#8801 = ORIENTED_EDGE ( 'NONE', *, *, #4949, .F. ) ;
#8802 = CARTESIAN_POINT ( 'NONE',  ( -1.135272562821090014, 28.49680007765648071, -3.311245368580554072 ) ) ;
#8803 = CYLINDRICAL_SURFACE ( 'NONE', #8050, 8.000000000000000000 ) ;
#8804 = CARTESIAN_POINT ( 'NONE',  ( 1.071796769724485232, -25.43924133869294835, -5.075734560980603050 ) ) ;
#8805 = PRESENTATION_STYLE_ASSIGNMENT (( #4833 ) ) ;
#8806 = ORIENTED_EDGE ( 'NONE', *, *, #1503, .F. ) ;
#8807 = AXIS2_PLACEMENT_3D ( 'NONE', #8329, #13904, #6935 ) ;
#8808 = CARTESIAN_POINT ( 'NONE',  ( 3.518350579753605434, 23.12819992234354416, -1.080741659609877114 ) ) ;
#8809 = CARTESIAN_POINT ( 'NONE',  ( 4.299564228933482956E-15, -23.15635672500629738, -15.76301181529063555 ) ) ;
#8810 = CIRCLE ( 'NONE', #13550, 2.000000000000001776 ) ;
#8811 = CARTESIAN_POINT ( 'NONE',  ( -4.243569643750000786, -21.80312760463873900, -6.856613161887861629 ) ) ;
#8812 = CARTESIAN_POINT ( 'NONE',  ( -2.500000000000001332, 17.99680007765648071, 0.05647727720535858364 ) ) ;
#8813 = CARTESIAN_POINT ( 'NONE',  ( -2.798362969681409851, 37.25319992234354061, -2.102939460078765421 ) ) ;
#8814 = CARTESIAN_POINT ( 'NONE',  ( 4.730628863548789710E-15, -22.79010942140499907, -16.80914949947612413 ) ) ;
#8815 = CARTESIAN_POINT ( 'NONE',  ( 1.533898589781675205E-14, -28.28997139934942595, -9.146999014867043698 ) ) ;
#8816 =( BOUNDED_CURVE ( )  B_SPLINE_CURVE ( 3, ( #5409, #14116, #16923, #6969 ),
 .UNSPECIFIED., .F., .T. ) 
 B_SPLINE_CURVE_WITH_KNOTS ( ( 4, 4 ),
 ( 5.253488506341834174, 6.283185307179586232 ),
 .UNSPECIFIED. ) 
 CURVE ( )  GEOMETRIC_REPRESENTATION_ITEM ( )  RATIONAL_B_SPLINE_CURVE ( ( 1.000000000000000000, 0.9135782535825734962, 0.9135782535825734962, 1.000000000000000000 ) ) 
 REPRESENTATION_ITEM ( '' )  );
#8817 = CARTESIAN_POINT ( 'NONE',  ( 4.243569643749996345, -24.25100835891830542, -6.081059070213228779 ) ) ;
#8818 = CARTESIAN_POINT ( 'NONE',  ( 0.000000000000000000, -3.999999999999991562, 11.59510085796834566 ) ) ;
#8819 = AXIS2_PLACEMENT_3D ( 'NONE', #1345, #7067, #12736 ) ;
#8820 = EDGE_CURVE ( 'NONE', #177, #9284, #3446, .T. ) ;
#8821 = AXIS2_PLACEMENT_3D ( 'NONE', #11066, #11606, #8824 ) ;
#8822 = CARTESIAN_POINT ( 'NONE',  ( -1.734723475976807094E-15, 36.39999999999999147, -2.500000000000000000 ) ) ;
#8823 = DIRECTION ( 'NONE',  ( -0.000000000000000000, -0.5735764363510414965, -0.8191520442889950182 ) ) ;
#8824 = DIRECTION ( 'NONE',  ( 0.000000000000000000, 0.8191520442889949072, -0.5735764363510414965 ) ) ;
#8825 = VERTEX_POINT ( 'NONE', #13617 ) ;
#8826 = EDGE_LOOP ( 'NONE', ( #16683, #9224, #14820, #13051 ) ) ;
#8827 = CARTESIAN_POINT ( 'NONE',  ( -4.243569643750000786, -21.28690881192279960, -6.119376322027766157 ) ) ;
#8828 = CARTESIAN_POINT ( 'NONE',  ( 10.00000000000000000, 31.99999999999999289, -2.500000000000003109 ) ) ;
#8829 = FACE_BOUND ( 'NONE', #9067, .T. ) ;
#8830 = ORIENTED_EDGE ( 'NONE', *, *, #14311, .T. ) ;
#8831 = CARTESIAN_POINT ( 'NONE',  ( -0.8262555684460826111, 24.00319992234354416, 2.360188852285421302 ) ) ;
#8832 = CARTESIAN_POINT ( 'NONE',  ( 4.730628863548789710E-15, -22.49973635050228538, -16.39445377705482088 ) ) ;
#8833 = CARTESIAN_POINT ( 'NONE',  ( 2.211161402132902243, 17.12180007765648071, 2.942372952327172442 ) ) ;
#8834 = CIRCLE ( 'NONE', #16556, 4.324969328314201000 ) ;
#8835 = LINE ( 'NONE', #4860, #12541 ) ;
#8836 = VECTOR ( 'NONE', #11580, 999.9999999999998863 ) ;
#8837 = CYLINDRICAL_SURFACE ( 'NONE', #1665, 4.000000000000000000 ) ;
#8838 = VERTEX_POINT ( 'NONE', #1299 ) ;
#8839 = CARTESIAN_POINT ( 'NONE',  ( -3.481649420246369697, 40.37180007765648071, 1.193696214020542490 ) ) ;
#8840 = CARTESIAN_POINT ( 'NONE',  ( 1.999999999999994449, -22.86087414489934488, -2.327754914381585660 ) ) ;
#8841 = FACE_OUTER_BOUND ( 'NONE', #2450, .T. ) ;
#8842 = CARTESIAN_POINT ( 'NONE',  ( -5.330712181944246111E-15, -29.62412893858816432, -9.483180404412477671 ) ) ;
#8843 = DIRECTION ( 'NONE',  ( -0.000000000000000000, -0.5735764363510414965, -0.8191520442889950182 ) ) ;
#8844 = CIRCLE ( 'NONE', #11502, 0.9999999999999991118 ) ;
#8845 = CARTESIAN_POINT ( 'NONE',  ( 1.533898589781675205E-14, -27.77375260663349366, -8.409762175006950002 ) ) ;
#8846 = CARTESIAN_POINT ( 'NONE',  ( -10.00000000000000178, 29.79999999999999716, -2.500000000000001776 ) ) ;
#8847 = CARTESIAN_POINT ( 'NONE',  ( 2.121784821875004390, -21.45984223041904926, -12.77358600641437469 ) ) ;
#8848 = CARTESIAN_POINT ( 'NONE',  ( -2.000000000000005773, -22.71031033106213570, -2.112727503762495296 ) ) ;
#8849 = CARTESIAN_POINT ( 'NONE',  ( 1.497042530366477164, 18.87180007765648071, -2.161531897785062384 ) ) ;
#8850 = EDGE_LOOP ( 'NONE', ( #7884, #9066, #5654, #5536 ) ) ;
#8851 = CARTESIAN_POINT ( 'NONE',  ( 2.115076519116362963, 21.37180007765647716, -3.012182706137107591 ) ) ;
#8852 = CARTESIAN_POINT ( 'NONE',  ( 1.071796769724485454, -21.10300825486137200, -12.83052629050617277 ) ) ;
#8853 = EDGE_CURVE ( 'NONE', #451, #7377, #931, .T. ) ;
#8854 = CARTESIAN_POINT ( 'NONE',  ( -4.000000000000004441, -27.98056965346157909, -11.65259680360067662 ) ) ;
#8855 = AXIS2_PLACEMENT_3D ( 'NONE', #3398, #14625, #14812 ) ;
#8856 = CARTESIAN_POINT ( 'NONE',  ( 4.000000000000000888, -23.33565214516171338, -9.045285029719133618 ) ) ;
#8857 = EDGE_CURVE ( 'NONE', #2215, #10311, #3790, .T. ) ;
#8858 = CARTESIAN_POINT ( 'NONE',  ( 3.500000000000000444, 20.75319992234354416, 0.05647727720529520379 ) ) ;
#8859 = EDGE_LOOP ( 'NONE', ( #15250, #17834, #15000, #3152 ) ) ;
#8860 = CARTESIAN_POINT ( 'NONE',  ( -5.330712181944246111E-15, -28.10773623498509721, -7.317547187323447666 ) ) ;
#8861 = EDGE_CURVE ( 'NONE', #13482, #9317, #13712, .T. ) ;
#8862 = AXIS2_PLACEMENT_3D ( 'NONE', #12565, #5251, #8388 ) ;
#8863 = CARTESIAN_POINT ( 'NONE',  ( 3.518350579753631191, 16.87180007765648071, 1.080741659609802285 ) ) ;
#8864 = VERTEX_POINT ( 'NONE', #12313 ) ;
#8865 = EDGE_CURVE ( 'NONE', #13697, #3107, #4310, .T. ) ;
#8866 = CARTESIAN_POINT ( 'NONE',  ( -4.000000000000007105, 6.938893903907228378E-15, 30.00000000000000000 ) ) ;
#8867 = CARTESIAN_POINT ( 'NONE',  ( -4.243569643750000786, -25.96514162091098399, -12.80058518325988182 ) ) ;
#8868 = DIRECTION ( 'NONE',  ( 0.000000000000000000, 0.000000000000000000, -1.000000000000000000 ) ) ;
#8869 = DIRECTION ( 'NONE',  ( -0.000000000000000000, -0.5735764363510414965, -0.8191520442889950182 ) ) ;
#8870 = DIRECTION ( 'NONE',  ( -0.000000000000000000, -0.5735764363510414965, -0.8191520442889950182 ) ) ;
#8871 = CARTESIAN_POINT ( 'NONE',  ( 2.121784821874994176, -25.01788001334084299, -5.040520239083123855 ) ) ;
#8872 = ADVANCED_FACE ( 'NONE', ( #9624 ), #2600, .F. ) ;
#8873 = ORIENTED_EDGE ( 'NONE', *, *, #4053, .T. ) ;
#8874 = CARTESIAN_POINT ( 'NONE',  ( -1.661723472263481630E-14, -21.60770034685848984, -13.55130129571035447 ) ) ;
#8875 = CARTESIAN_POINT ( 'NONE',  ( -1.734723475976807094E-15, 34.19999999999999574, -2.500000000000000000 ) ) ;
#8876 = CIRCLE ( 'NONE', #3272, 8.000000000000001776 ) ;
#8877 = CARTESIAN_POINT ( 'NONE',  ( 4.000000000000003553, -21.16428301933063949, -9.970566447840647939 ) ) ;
#8878 = ORIENTED_EDGE ( 'NONE', *, *, #1348, .F. ) ;
#8879 = VERTEX_POINT ( 'NONE', #12947 ) ;
#8880 = CARTESIAN_POINT ( 'NONE',  ( 1.071796769724494780, -27.50411650955668463, -8.024681920420986714 ) ) ;
#8881 = DIRECTION ( 'NONE',  ( 0.000000000000000000, 0.000000000000000000, -1.000000000000000000 ) ) ;
#8882 = CARTESIAN_POINT ( 'NONE',  ( 4.518350579753602325, 25.62819992234354416, -1.405661355842793725 ) ) ;
#8883 = CARTESIAN_POINT ( 'NONE',  ( 2.864755990943222308, 28.00319992234354416, -2.011557305968548093 ) ) ;
#8884 = CARTESIAN_POINT ( 'NONE',  ( 1.989345975306457071, 23.50319992234355126, 1.515154207786300500 ) ) ;
#8885 = ORIENTED_EDGE ( 'NONE', *, *, #3365, .F. ) ;
#8886 = CARTESIAN_POINT ( 'NONE',  ( -1.336863392178478716, 17.49680007765647716, 4.297206761780677731 ) ) ;
#8887 = CARTESIAN_POINT ( 'NONE',  ( -2.000000000000005773, -24.71065815213145100, -4.969520257213599024 ) ) ;
#8888 = VERTEX_POINT ( 'NONE', #5637 ) ;
#8889 = AXIS2_PLACEMENT_3D ( 'NONE', #14648, #16132, #15507 ) ;
#8890 = DIRECTION ( 'NONE',  ( -3.373073425510457965E-16, 0.000000000000000000, -1.000000000000000000 ) ) ;
#8891 = CARTESIAN_POINT ( 'NONE',  ( 1.027846397803542144, 31.24680007765647716, -3.346150245485522312 ) ) ;
#8892 = CARTESIAN_POINT ( 'NONE',  ( -9.974300771894275996, -9.920519257017851089, 4.129833639286026425 ) ) ;
#8893 =( REPRESENTATION_RELATIONSHIP ('NONE','NONE', #15868, #7684 ) REPRESENTATION_RELATIONSHIP_WITH_TRANSFORMATION ( #2569 )SHAPE_REPRESENTATION_RELATIONSHIP( ) );
#8894 = CARTESIAN_POINT ( 'NONE',  ( 2.121784821874994176, -24.72750694243812219, -4.625824516661818819 ) ) ;
#8895 = CARTESIAN_POINT ( 'NONE',  ( 0.05938372350929014415, 29.87180007765647005, 4.731580009072201776 ) ) ;
#8896 = ORIENTED_EDGE ( 'NONE', *, *, #964, .T. ) ;
#8897 = CARTESIAN_POINT ( 'NONE',  ( -1.027846397803541700, 32.49680007765648071, 3.346150245485522312 ) ) ;
#8898 = DIRECTION ( 'NONE',  ( -1.000000000000000000, -0.000000000000000000, -0.000000000000000000 ) ) ;
#8899 = DIRECTION ( 'NONE',  ( 0.000000000000000000, 0.8191520442889952403, -0.5735764363510413855 ) ) ;
#8900 = CARTESIAN_POINT ( 'NONE',  ( 9.000000000000005329, -10.00000000000000000, 15.14468620625654616 ) ) ;
#8901 = CARTESIAN_POINT ( 'NONE',  ( 0.000000000000000000, 20.99999999999999289, 2.500000000000000000 ) ) ;
#8902 = EDGE_LOOP ( 'NONE', ( #16516, #3621 ) ) ;
#8903 = VECTOR ( 'NONE', #452, 1000.000000000000000 ) ;
#8904 = CARTESIAN_POINT ( 'NONE',  ( -3.481649420246394122, 29.62819992234353350, -1.193696214020467883 ) ) ;
#8905 = CARTESIAN_POINT ( 'NONE',  ( -1.734723475976807094E-15, 25.39999999999999503, -2.500000000000000000 ) ) ;
#8906 = CARTESIAN_POINT ( 'NONE',  ( 2.121784821875004390, -18.87874826683935936, -9.087401807113897334 ) ) ;
#8907 = CARTESIAN_POINT ( 'NONE',  ( -0.7188294034286043521, 24.99680007765647716, 2.395093729190366005 ) ) ;
#8908 = CIRCLE ( 'NONE', #7126, 0.9999999999999991118 ) ;
#8909 = VECTOR ( 'NONE', #8325, 1000.000000000000000 ) ;
#8910 = CARTESIAN_POINT ( 'NONE',  ( 3.500000000000000444, 33.25319992234354771, 0.05647727720529520379 ) ) ;
#8911 = CARTESIAN_POINT ( 'NONE',  ( 4.243569643750000786, -26.61041511180591357, -13.72213123308499760 ) ) ;
#8912 = CARTESIAN_POINT ( 'NONE',  ( -3.999999999999997335, -24.94988749924751303, -15.37696994014802065 ) ) ;
#8913 = CARTESIAN_POINT ( 'NONE',  ( -2.121784821875005722, -25.83522643514106676, -6.207811902194944054 ) ) ;
#8914 = CARTESIAN_POINT ( 'NONE',  ( -7.037433860066684588, -13.81827297165700408, -0.01215148577350405948 ) ) ;
#8915 = CARTESIAN_POINT ( 'NONE',  ( -6.262826437386821432, -14.35615764868811617, -3.437201991565423054 ) ) ;
#8916 = CARTESIAN_POINT ( 'NONE',  ( -5.577813053751546416E-15, -23.57947491511155036, -2.419712850136908511 ) ) ;
#8917 = DIRECTION ( 'NONE',  ( -4.915049848600951133E-16, 0.000000000000000000, -1.000000000000000000 ) ) ;
#8918 = ORIENTED_EDGE ( 'NONE', *, *, #8679, .T. ) ;
#8919 = ORIENTED_EDGE ( 'NONE', *, *, #14586, .F. ) ;
#8920 = CARTESIAN_POINT ( 'NONE',  ( -1.734723475976807094E-15, 18.79999999999999361, -2.500000000000000000 ) ) ;
#8921 = CARTESIAN_POINT ( 'NONE',  ( -6.938893903907228378E-15, 6.938893903907228378E-15, -30.00000000000000000 ) ) ;
#8922 = ORIENTED_EDGE ( 'NONE', *, *, #15717, .F. ) ;
#8923 = CARTESIAN_POINT ( 'NONE',  ( -1.497042530366522461, 29.87819992234354416, -2.161531897785030409 ) ) ;
#8924 =( LENGTH_UNIT ( ) NAMED_UNIT ( * ) SI_UNIT ( .MILLI., .METRE. ) );
#8925 = CARTESIAN_POINT ( 'NONE',  ( 4.243569643750003451, -23.77537026298940148, -13.94475769486455619 ) ) ;
#8926 = CARTESIAN_POINT ( 'NONE',  ( -4.000000000000007105, 0.000000000000000000, 30.00000000000000000 ) ) ;
#8927 =( BOUNDED_CURVE ( )  B_SPLINE_CURVE ( 3, ( #6620, #13656, #12265, #2734 ),
 .UNSPECIFIED., .F., .T. ) 
 B_SPLINE_CURVE_WITH_KNOTS ( ( 4, 4 ),
 ( -8.881784197001252323E-16, 1.570796326794896558 ),
 .UNSPECIFIED. ) 
 CURVE ( )  GEOMETRIC_REPRESENTATION_ITEM ( )  RATIONAL_B_SPLINE_CURVE ( ( 1.000000000000000000, 0.8047378541243648264, 0.8047378541243648264, 1.000000000000000000 ) ) 
 REPRESENTATION_ITEM ( '' )  );
#8928 = MECHANICAL_DESIGN_GEOMETRIC_PRESENTATION_REPRESENTATION (  '', ( #11896 ), #956 ) ;
#8929 = DIRECTION ( 'NONE',  ( 3.469446951953612217E-16, -0.000000000000000000, 1.000000000000000000 ) ) ;
#8930 = EDGE_CURVE ( 'NONE', #3107, #13697, #16471, .T. ) ;
#8931 = CARTESIAN_POINT ( 'NONE',  ( -0.9156706748235758919, -10.00000000000091660, -4.445527249945649295 ) ) ;
#8932 = ORIENTED_EDGE ( 'NONE', *, *, #14311, .F. ) ;
#8933 = DIRECTION ( 'NONE',  ( -0.000000000000000000, -1.000000000000000000, -0.000000000000000000 ) ) ;
#8934 = CARTESIAN_POINT ( 'NONE',  ( -5.279047395330986450E-15, -23.57014917145950506, -1.327545676256177254 ) ) ;
#8935 = VECTOR ( 'NONE', #6579, 1000.000000000000114 ) ;
#8936 = CARTESIAN_POINT ( 'NONE',  ( -3.999999999999997335, -22.36879353566782314, -11.69078574084754152 ) ) ;
#8937 = COLOUR_RGB ( '',0.8941176470588234615, 0.8941176470588234615, 0.8941176470588234615 ) ;
#8938 = CARTESIAN_POINT ( 'NONE',  ( -4.243569643750004339, -26.11154692433198576, -8.738183513875661390 ) ) ;
#8939 = CARTESIAN_POINT ( 'NONE',  ( 4.898587196589413815E-16, 2.700915433685006750, 35.11257424290206330 ) ) ;
#8940 = AXIS2_PLACEMENT_3D ( 'NONE', #17773, #16090, #14701 ) ;
#8941 = CARTESIAN_POINT ( 'NONE',  ( 8.500000000000019540, 0.000000000000000000, -22.49999999999999289 ) ) ;
#8942 = FACE_OUTER_BOUND ( 'NONE', #14157, .T. ) ;
#8943 = CARTESIAN_POINT ( 'NONE',  ( 2.121784821875004390, -19.91118585227123816, -10.56187548683408828 ) ) ;
#8944 = CARTESIAN_POINT ( 'NONE',  ( 5.040478647146458435, -15.02265568887750469, -7.935421837999466099 ) ) ;
#8945 = DIRECTION ( 'NONE',  ( 0.000000000000000000, -0.5000000000000011102, -0.8660254037844380415 ) ) ;
#8946 = CARTESIAN_POINT ( 'NONE',  ( 0.8262555684461332373, 24.74680007765647716, 2.360188852285403982 ) ) ;
#8947 = EDGE_LOOP ( 'NONE', ( #2313, #15482, #847, #9516 ) ) ;
#8948 = CARTESIAN_POINT ( 'NONE',  ( 2.864755990943265829, 24.49680007765647716, 2.011557305968487697 ) ) ;
#8949 = CARTESIAN_POINT ( 'NONE',  ( 4.000000000000003553, -22.51935735091492674, -11.90581315348016567 ) ) ;
#8950 = AXIS2_PLACEMENT_3D ( 'NONE', #10433, #11916, #4963 ) ;
#8951 = SURFACE_STYLE_FILL_AREA ( #3404 ) ;
#8952 = CARTESIAN_POINT ( 'NONE',  ( 3.999999999999996447, -28.15264258436690525, -11.89834241688737393 ) ) ;
#8953 = VECTOR ( 'NONE', #4616, 1000.000000000000000 ) ;
#8954 = CARTESIAN_POINT ( 'NONE',  ( 8.500000000000019540, 10.00000000000000000, -22.49999999999999289 ) ) ;
#8955 = CARTESIAN_POINT ( 'NONE',  ( 0.05938372350920109732, 15.12819992234354238, -3.680117784833935701 ) ) ;
#8956 = EDGE_LOOP ( 'NONE', ( #6118, #6421, #17254, #16026, #9135 ) ) ;
#8957 = CARTESIAN_POINT ( 'NONE',  ( -2.121784821874996396, -20.15854069044762298, -10.91513480593371987 ) ) ;
#8958 = CARTESIAN_POINT ( 'NONE',  ( -2.733110507866247652, 37.62180007765646650, 3.862833514489154574 ) ) ;
#8959 = CIRCLE ( 'NONE', #10123, 2.200000000000000622 ) ;
#8960 = ORIENTED_EDGE ( 'NONE', *, *, #12288, .F. ) ;
#8961 = DIRECTION ( 'NONE',  ( -1.000000000000000000, 0.000000000000000000, 4.336808689942021680E-16 ) ) ;
#8962 = CARTESIAN_POINT ( 'NONE',  ( 8.499999999999992895, 14.80000000000000071, 18.29999999999999716 ) ) ;
#8963 = ADVANCED_FACE ( 'NONE', ( #15652 ), #11552, .T. ) ;
#8964 = CARTESIAN_POINT ( 'NONE',  ( -4.243569643750000786, -25.70703222455301784, -12.43196676332983408 ) ) ;
#8965 = LINE ( 'NONE', #15809, #1077 ) ;
#8966 = VECTOR ( 'NONE', #8041, 1000.000000000000000 ) ;
#8967 = EDGE_CURVE ( 'NONE', #1285, #15329, #8165, .T. ) ;
#8968 = CARTESIAN_POINT ( 'NONE',  ( -1.071796769724491671, -22.62861123157153287, -15.00931314077462631 ) ) ;
#8969 = AXIS2_PLACEMENT_3D ( 'NONE', #4831, #4918, #13166 ) ;
#8970 = EDGE_CURVE ( 'NONE', #935, #5386, #2278, .T. ) ;
#8971 = CARTESIAN_POINT ( 'NONE',  ( -1.661723472263481630E-14, -21.80128239342201724, -13.82776510965112671 ) ) ;
#8972 = CARTESIAN_POINT ( 'NONE',  ( -4.243569643749997233, -18.04319075220617563, -5.758356952251413752 ) ) ;
#8973 = ORIENTED_EDGE ( 'NONE', *, *, #6778, .F. ) ;
#8974 = CARTESIAN_POINT ( 'NONE',  ( -3.999999999999997335, -22.94953967817819773, -12.52017718669691604 ) ) ;
#8975 = CARTESIAN_POINT ( 'NONE',  ( 4.000000000000000888, -23.40017949495614857, -9.137439635708412666 ) ) ;
#8976 = FACE_OUTER_BOUND ( 'NONE', #15658, .T. ) ;
#8977 = VERTEX_POINT ( 'NONE', #11649 ) ;
#8978 = ORIENTED_EDGE ( 'NONE', *, *, #5352, .F. ) ;
#8979 = DIRECTION ( 'NONE',  ( 0.000000000000000000, 0.8191520442889952403, -0.5735764363510413855 ) ) ;
#8980 = DIRECTION ( 'NONE',  ( 1.000000000000000000, 0.000000000000000000, 0.000000000000000000 ) ) ;
#8981 = SHAPE_REPRESENTATION_RELATIONSHIP ( 'NONE' , 'NONE' ,  #5199, #9153 ) ;
#8982 = EDGE_CURVE ( 'NONE', #15831, #12442, #1385, .T. ) ;
#8983 = CARTESIAN_POINT ( 'NONE',  ( -0.05938372350918959958, 26.37819992234355126, 4.731580009072201776 ) ) ;
#8984 = CARTESIAN_POINT ( 'NONE',  ( -2.864755990943222308, 36.75319992234354061, 2.011557305968548093 ) ) ;
#8985 = CARTESIAN_POINT ( 'NONE',  ( -2.055738996568281518, 16.75319992234354416, 1.423772053676066962 ) ) ;
#8986 = AXIS2_PLACEMENT_3D ( 'NONE', #10340, #3676, #2022 ) ;
#8987 = ORIENTED_EDGE ( 'NONE', *, *, #7959, .F. ) ;
#8988 = CARTESIAN_POINT ( 'NONE',  ( -4.499999999999999112, 39.50319992234354061, -0.05647727720528529505 ) ) ;
#8989 = CARTESIAN_POINT ( 'NONE',  ( -3.999999999999997335, -20.56202776116204234, -9.110456801337207366 ) ) ;
#8990 = SHAPE_REPRESENTATION ( 'Plunger', ( #16940 ), #5661 ) ;
#8991 = VERTEX_POINT ( 'NONE', #8411 ) ;
#8992 = DIRECTION ( 'NONE',  ( -0.000000000000000000, -1.000000000000000000, -0.000000000000000000 ) ) ;
#8993 = CARTESIAN_POINT ( 'NONE',  ( 0.05938372350927906274, 32.37180007765647360, 3.680117784833935701 ) ) ;
#8994 = DIRECTION ( 'NONE',  ( 0.000000000000000000, 0.000000000000000000, -1.000000000000000000 ) ) ;
#8995 = CARTESIAN_POINT ( 'NONE',  ( -4.243569643750000786, -22.06123700099670870, -7.225231581817909365 ) ) ;
#8996 = EDGE_CURVE ( 'NONE', #11449, #5080, #18325, .T. ) ;
#8997 = CARTESIAN_POINT ( 'NONE',  ( -4.499999999999999112, 30.49680007765648071, 0.05647727720537927543 ) ) ;
#8998 = CARTESIAN_POINT ( 'NONE',  ( 3.250762944584260072, -21.87258937905581746, -2.200190645090608133 ) ) ;
#8999 = EDGE_LOOP ( 'NONE', ( #11746, #800, #12211, #5173 ) ) ;
#9000 = CARTESIAN_POINT ( 'NONE',  ( 1.135272562821090458, 29.74680007765647716, 3.311245368580554072 ) ) ;
#9001 = CARTESIAN_POINT ( 'NONE',  ( -3.678256433394857527, -9.999999999999056755, 21.51556408012798371 ) ) ;
#9002 = CARTESIAN_POINT ( 'NONE',  ( -1.734723475976807094E-15, 36.39999999999999147, -2.500000000000000000 ) ) ;
#9003 = CYLINDRICAL_SURFACE ( 'NONE', #7155, 0.9999999999999991118 ) ;
#9004 =( NAMED_UNIT ( * ) PLANE_ANGLE_UNIT ( ) SI_UNIT ( $, .RADIAN. ) );
#9005 = VERTEX_POINT ( 'NONE', #4518 ) ;
#9006 = CARTESIAN_POINT ( 'NONE',  ( 2.211161402132839626, 27.87819992234354061, -2.942372952327218183 ) ) ;
#9007 = CARTESIAN_POINT ( 'NONE',  ( 9.000000000000005329, 29.79999999999999716, 2.499999999999997335 ) ) ;
#9008 = CARTESIAN_POINT ( 'NONE',  ( 4.730628863548789710E-15, -17.59565781970087883, -9.390703798383910339 ) ) ;
#9009 = CARTESIAN_POINT ( 'NONE',  ( 1.593127413382998903, 19.62180007765648071, 2.091722143975139669 ) ) ;
#9010 = CARTESIAN_POINT ( 'NONE',  ( 1.444289557195957086, 15.25319992234354594, -4.262301884875733471 ) ) ;
#9011 = DIRECTION ( 'NONE',  ( 0.000000000000000000, -0.5735764363510413855, -0.8191520442889951292 ) ) ;
#9012 = CARTESIAN_POINT ( 'NONE',  ( -5.279047395330986450E-15, -30.53910287312466210, -11.28024301436746768 ) ) ;
#9013 = CARTESIAN_POINT ( 'NONE',  ( -5.330712181944245322E-15, -25.52664227140541797, -3.631362988022969862 ) ) ;
#9014 = CARTESIAN_POINT ( 'NONE',  ( -6.428571428571425272, -14.26578344203648285, -2.827263138854410496 ) ) ;
#9015 = CARTESIAN_POINT ( 'NONE',  ( 0.000000000000000000, -1.759474945355381292, 3.047500000000002540 ) ) ;
#9016 = CARTESIAN_POINT ( 'NONE',  ( -1.071796769724496334, -21.53164629634521887, -13.44268485506515809 ) ) ;
#9017 = VERTEX_POINT ( 'NONE', #15838 ) ;
#9018 = EDGE_LOOP ( 'NONE', ( #15938, #6781 ) ) ;
#9019 = CARTESIAN_POINT ( 'NONE',  ( -1.071796769724486786, -16.43398571898028138, -6.162471062453482418 ) ) ;
#9020 = CARTESIAN_POINT ( 'NONE',  ( 12.00000000000000178, 48.00000000000000000, -15.00000000000000000 ) ) ;
#9021 = CARTESIAN_POINT ( 'NONE',  ( -14.99999999999999645, -10.00000000000000000, 30.00000000000000000 ) ) ;
#9022 = VERTEX_POINT ( 'NONE', #8674 ) ;
#9023 = CARTESIAN_POINT ( 'NONE',  ( 1.497042530366522461, 26.12819992234354416, 2.161531897785029965 ) ) ;
#9024 = CARTESIAN_POINT ( 'NONE',  ( 0.000000000000000000, 0.000000000000000000, 0.000000000000000000 ) ) ;
#9025 = CARTESIAN_POINT ( 'NONE',  ( 2.121784821874994176, -28.08292909509171764, -9.417863975752439387 ) ) ;
#9026 = CARTESIAN_POINT ( 'NONE',  ( -2.211161402132902243, 20.87180007765647716, -2.942372952327172886 ) ) ;
#9027 = PLANE ( 'NONE',  #8684 ) ;
#9028 = CARTESIAN_POINT ( 'NONE',  ( 0.000000000000000000, 27.59999999999999432, 2.500000000000000000 ) ) ;
#9029 = CARTESIAN_POINT ( 'NONE',  ( -4.243569643750005227, -27.95057637338251411, -11.36458975587725106 ) ) ;
#9030 = ADVANCED_FACE ( 'NONE', ( #4603 ), #11368, .F. ) ;
#9031 = CARTESIAN_POINT ( 'NONE',  ( 1.475796370471763337E-14, -21.86580974321645598, -13.91991971564040220 ) ) ;
#9032 = CARTESIAN_POINT ( 'NONE',  ( 4.243569643750003451, -21.71049509212565454, -10.99581033542417252 ) ) ;
#9033 = CARTESIAN_POINT ( 'NONE',  ( 1.071796769724504328, -23.05172942167677519, -1.666014175620901705 ) ) ;
#9034 = EDGE_CURVE ( 'NONE', #17537, #7005, #13195, .T. ) ;
#9035 = CARTESIAN_POINT ( 'NONE',  ( 8.000000000000005329, 25.39999999999999503, 2.499999999999997780 ) ) ;
#9036 = EDGE_CURVE ( 'NONE', #13551, #1052, #4434, .T. ) ;
#9037 = FACE_OUTER_BOUND ( 'NONE', #12762, .T. ) ;
#9038 = CARTESIAN_POINT ( 'NONE',  ( 4.243569643750000786, -22.96461988824960443, -8.515396051573073777 ) ) ;
#9039 = DIRECTION ( 'NONE',  ( 0.000000000000000000, 0.000000000000000000, -1.000000000000000000 ) ) ;
#9040 = ADVANCED_FACE ( 'NONE', ( #10065 ), #15562, .F. ) ;
#9041 = CARTESIAN_POINT ( 'NONE',  ( -8.500000000000005329, 13.00000000000000178, -20.49999999999999645 ) ) ;
#9042 = CARTESIAN_POINT ( 'NONE',  ( -0.7188294034286043521, 32.49680007765648782, 2.395093729190366005 ) ) ;
#9043 = ORIENTED_EDGE ( 'NONE', *, *, #85, .T. ) ;
#9044 = CARTESIAN_POINT ( 'NONE',  ( 3.500000000000000444, 26.74680007765648071, -0.05647727720536935281 ) ) ;
#9045 = DIRECTION ( 'NONE',  ( -0.000000000000000000, -1.000000000000000000, -0.000000000000000000 ) ) ;
#9046 = APPLICATION_PROTOCOL_DEFINITION ( 'draft international standard', 'automotive_design', 1998, #264 ) ;
#9047 = CARTESIAN_POINT ( 'NONE',  ( 4.000000000000000888, -25.20694526946192937, -11.71776857521874504 ) ) ;
#9048 = DIRECTION ( 'NONE',  ( 1.000000000000000000, 0.000000000000000000, -8.673617379884034239E-17 ) ) ;
#9049 = CARTESIAN_POINT ( 'NONE',  ( -1.027846397803611866, 20.00319992234354416, -3.346150245485499219 ) ) ;
#9050 = ORIENTED_EDGE ( 'NONE', *, *, #13460, .T. ) ;
#9051 = CARTESIAN_POINT ( 'NONE',  ( 2.121784821875004390, -19.68534013045801956, -10.23933436939529606 ) ) ;
#9052 = CARTESIAN_POINT ( 'NONE',  ( 3.607379964056306676, 38.99680007765648071, -2.690724712371305838 ) ) ;
#9053 = ORIENTED_EDGE ( 'NONE', *, *, #13852, .F. ) ;
#9054 = CIRCLE ( 'NONE', #16780, 4.000000000000001776 ) ;
#9055 = VECTOR ( 'NONE', #16510, 1000.000000000000000 ) ;
#9056 = CARTESIAN_POINT ( 'NONE',  ( 4.000000000000000000, 3.518949890710770134, -4.119968255444916849E-15 ) ) ;
#9057 = CARTESIAN_POINT ( 'NONE',  ( -4.243569643750005227, -27.69246697702454441, -10.99597133594720333 ) ) ;
#9058 = DIRECTION ( 'NONE',  ( 0.000000000000000000, 0.000000000000000000, -1.000000000000000000 ) ) ;
#9059 = CARTESIAN_POINT ( 'NONE',  ( 10.00000000000000000, 38.59999999999999432, -2.500000000000003109 ) ) ;
#9060 = CARTESIAN_POINT ( 'NONE',  ( 0.000000000000000000, -10.00099999999999767, 4.000000000000000000 ) ) ;
#9061 = CARTESIAN_POINT ( 'NONE',  ( 4.243569643750000786, -26.83626083361913217, -14.04467235052378804 ) ) ;
#9062 = ORIENTED_EDGE ( 'NONE', *, *, #8706, .T. ) ;
#9063 = CARTESIAN_POINT ( 'NONE',  ( -2.000000000000005773, -27.61438886186354225, -9.116477482433401391 ) ) ;
#9064 = CARTESIAN_POINT ( 'NONE',  ( -1.999999999999996225, -19.96029831712264979, -10.26425704877356715 ) ) ;
#9065 = CARTESIAN_POINT ( 'NONE',  ( 8.500000000000001776, 15.00000000000000000, -20.49999999999999645 ) ) ;
#9066 = ORIENTED_EDGE ( 'NONE', *, *, #15843, .T. ) ;
#9067 = EDGE_LOOP ( 'NONE', ( #2481, #15038, #13597, #9733 ) ) ;
#9068 = FACE_OUTER_BOUND ( 'NONE', #17516, .T. ) ;
#9069 = DIRECTION ( 'NONE',  ( -0.3258630558627247376, -2.016891894289822030E-15, 0.9454169814551708351 ) ) ;
#9070 = CARTESIAN_POINT ( 'NONE',  ( 4.481649420246397675, 25.87819992234355126, 1.518615910253363177 ) ) ;
#9071 = CARTESIAN_POINT ( 'NONE',  ( -1.135272562821019626, 34.00319992234354771, 3.311245368580577164 ) ) ;
#9072 = CARTESIAN_POINT ( 'NONE',  ( 2.500000000000001332, 20.75319992234354771, 0.05647727720530566764 ) ) ;
#9073 = ORIENTED_EDGE ( 'NONE', *, *, #718, .T. ) ;
#9074 = CARTESIAN_POINT ( 'NONE',  ( -2.733110507866247652, 20.12180007765647716, 3.862833514489154574 ) ) ;
#9075 = CARTESIAN_POINT ( 'NONE',  ( -4.000000000000004441, -23.78629196193964646, -5.662547478730636463 ) ) ;
#9076 = VERTEX_POINT ( 'NONE', #2859 ) ;
#9077 = EDGE_CURVE ( 'NONE', #13832, #15656, #8492, .T. ) ;
#9078 = CARTESIAN_POINT ( 'NONE',  ( 7.960204194457794491E-16, 13.00000000000000178, 6.499999999999999112 ) ) ;
#9079 = FILL_AREA_STYLE_COLOUR ( '', #6169 ) ;
#9080 = CARTESIAN_POINT ( 'NONE',  ( 3.999999999999996447, -27.31378704549856451, -10.70033255110795167 ) ) ;
#9081 = CARTESIAN_POINT ( 'NONE',  ( 4.730628863548789710E-15, -16.82132963062697684, -8.284848538593767131 ) ) ;
#9082 = AXIS2_PLACEMENT_3D ( 'NONE', #4020, #12729, #4290 ) ;
#9083 = CARTESIAN_POINT ( 'NONE',  ( 2.121784821874994176, -26.56653639148865409, -7.252230758663410271 ) ) ;
#9084 = CARTESIAN_POINT ( 'NONE',  ( 3.604268994871578258, -25.13996932480225155, -16.02211701335336258 ) ) ;
#9085 = ORIENTED_EDGE ( 'NONE', *, *, #10452, .T. ) ;
#9086 = CARTESIAN_POINT ( 'NONE',  ( 5.526342620815748674, -10.00000000000108713, 19.09106094340506132 ) ) ;
#9087 = DIRECTION ( 'NONE',  ( -0.000000000000000000, -1.000000000000000000, -0.000000000000000000 ) ) ;
#9088 = CARTESIAN_POINT ( 'NONE',  ( 2.343145750507616754, -3.999999999999992450, 25.54267522293724113 ) ) ;
#9089 = CARTESIAN_POINT ( 'NONE',  ( 4.243569643750000786, -27.12663390452184942, -14.45936807294509308 ) ) ;
#9090 = EDGE_LOOP ( 'NONE', ( #17618, #14196, #16794, #8058 ) ) ;
#9091 = CARTESIAN_POINT ( 'NONE',  ( -0.05938372350920063936, 26.37819992234354061, 3.680117784833935701 ) ) ;
#9092 = CARTESIAN_POINT ( 'NONE',  ( -15.00000000000000178, 10.00000000000000000, -25.00000000000000355 ) ) ;
#9093 = CARTESIAN_POINT ( 'NONE',  ( 4.243569643750000786, -21.15785411374382363, -5.935067112062737849 ) ) ;
#9094 = CARTESIAN_POINT ( 'NONE',  ( -2.055738996568313048, 23.24680007765648071, -1.423772053676023441 ) ) ;
#9095 = ADVANCED_FACE ( 'NONE', ( #1474 ), #5793, .F. ) ;
#9096 = CARTESIAN_POINT ( 'NONE',  ( 2.733110507866328920, 21.12819992234354416, 3.862833514489095510 ) ) ;
#9097 = CARTESIAN_POINT ( 'NONE',  ( 4.000000000000003553, -17.87338821647148990, -5.270681594739305531 ) ) ;
#9098 = EDGE_CURVE ( 'NONE', #6560, #17921, #7657, .T. ) ;
#9099 = CIRCLE ( 'NONE', #1115, 8.000000000000003553 ) ;
#9100 = CARTESIAN_POINT ( 'NONE',  ( 4.713407268011036227E-15, -22.58493632614797164, -16.02578754332199651 ) ) ;
#9101 = EDGE_CURVE ( 'NONE', #17559, #14256, #6345, .T. ) ;
#9102 = CARTESIAN_POINT ( 'NONE',  ( -2.121784821875005722, -24.54467945335122536, -4.364719802544705374 ) ) ;
#9103 = CARTESIAN_POINT ( 'NONE',  ( -7.471284260961007284, -13.12030862272409237, 4.270667233515101024 ) ) ;
#9104 = CARTESIAN_POINT ( 'NONE',  ( -1.999999999999996225, -22.73497432726586709, -14.22690506201481853 ) ) ;
#9105 = CARTESIAN_POINT ( 'NONE',  ( 1.071796769724476128, -16.90873056333943936, -6.840476965636138829 ) ) ;
#9106 = AXIS2_PLACEMENT_3D ( 'NONE', #5331, #6194, #11844 ) ;
#9107 = CARTESIAN_POINT ( 'NONE',  ( 1.071796769724495224, -19.29624248035560896, -10.25019735099583862 ) ) ;
#9108 = AXIS2_PLACEMENT_3D ( 'NONE', #14371, #1673, #4446 ) ;
#9109 = ORIENTED_EDGE ( 'NONE', *, *, #16020, .T. ) ;
#9110 = TOROIDAL_SURFACE ( 'NONE', #3493, 9.000000000000001776, 0.9999999999999991118 ) ;
#9111 = ORIENTED_EDGE ( 'NONE', *, *, #16594, .T. ) ;
#9112 = CARTESIAN_POINT ( 'NONE',  ( -3.999999999999997335, -17.78735175101882859, -5.147808788095962207 ) ) ;
#9113 = CARTESIAN_POINT ( 'NONE',  ( 1.071796769724495224, -17.42494935605538942, -7.577713805496229860 ) ) ;
#9114 = CARTESIAN_POINT ( 'NONE',  ( 4.000000000000000000, 4.506943796211476502E-15, 3.047499999999998987 ) ) ;
#9115 = ORIENTED_EDGE ( 'NONE', *, *, #14732, .F. ) ;
#9116 = CARTESIAN_POINT ( 'NONE',  ( -2.481649420246391902, 24.62819992234354416, -0.8687765177875723666 ) ) ;
#9117 = CARTESIAN_POINT ( 'NONE',  ( 2.121784821875004390, -22.23417041949295481, -13.87944126620451790 ) ) ;
#9118 = CARTESIAN_POINT ( 'NONE',  ( 3.481649420246369697, 21.62180007765647360, -1.193696214020541824 ) ) ;
#9119 = FACE_BOUND ( 'NONE', #13379, .T. ) ;
#9120 = DIRECTION ( 'NONE',  ( -0.000000000000000000, -1.000000000000000000, -0.000000000000000000 ) ) ;
#9121 = AXIS2_PLACEMENT_3D ( 'NONE', #15249, #2544, #6339 ) ;
#9122 = CARTESIAN_POINT ( 'NONE',  ( -4.243569643750005227, -27.69246697702454441, -10.99597133594720333 ) ) ;
#9123 = CIRCLE ( 'NONE', #16849, 0.9999999999999991118 ) ;
#9124 =( NAMED_UNIT ( * ) PLANE_ANGLE_UNIT ( ) SI_UNIT ( $, .RADIAN. ) );
#9125 = CARTESIAN_POINT ( 'NONE',  ( -2.121784821874996396, -21.41682399769271328, -12.71214960309270303 ) ) ;
#9126 = CARTESIAN_POINT ( 'NONE',  ( 4.146003165456281003, -26.80775609498953926, -14.74331408136821864 ) ) ;
#9127 = CARTESIAN_POINT ( 'NONE',  ( -10.00000000000000178, 36.39999999999999147, -2.500000000000001776 ) ) ;
#9128 = CARTESIAN_POINT ( 'NONE',  ( -1.734723475976807094E-15, 29.79999999999999716, -2.500000000000000000 ) ) ;
#9129 = CARTESIAN_POINT ( 'NONE',  ( -4.243569643750005227, -25.85343752797401606, -8.369565093945613654 ) ) ;
#9130 = ORIENTED_EDGE ( 'NONE', *, *, #31, .F. ) ;
#9131 = CARTESIAN_POINT ( 'NONE',  ( 0.000000000000000000, 5.977523610840987267, 32.81826849749789687 ) ) ;
#9132 = DIRECTION ( 'NONE',  ( 0.000000000000000000, 0.9936001553129349961, 0.1129545544106631688 ) ) ;
#9133 = CARTESIAN_POINT ( 'NONE',  ( -0.8262555684461330152, 28.49680007765648071, -2.360188852285403982 ) ) ;
#9134 = CIRCLE ( 'NONE', #5874, 0.9999999999999991118 ) ;
#9135 = ORIENTED_EDGE ( 'NONE', *, *, #7424, .T. ) ;
#9136 = CARTESIAN_POINT ( 'NONE',  ( 1.135272562821090458, 27.24680007765648071, 3.311245368580554072 ) ) ;
#9137 = CARTESIAN_POINT ( 'NONE',  ( -1.661723472263481630E-14, -20.57526276142661459, -12.07682761599016175 ) ) ;
#9138 = DIRECTION ( 'NONE',  ( -0.000000000000000000, -1.000000000000000000, -0.000000000000000000 ) ) ;
#9139 = CARTESIAN_POINT ( 'NONE',  ( -2.115076519116425580, 22.37819992234353350, -3.012182706137062738 ) ) ;
#9140 = ADVANCED_FACE ( 'NONE', ( #13326 ), #16031, .F. ) ;
#9141 = APPLICATION_CONTEXT ( 'automotive_design' ) ;
#9142 = EDGE_LOOP ( 'NONE', ( #17848, #11372, #15956, #14922 ) ) ;
#9143 = CARTESIAN_POINT ( 'NONE',  ( -4.243569643750004339, -24.85326361708688836, -6.941168716716676457 ) ) ;
#9144 = CARTESIAN_POINT ( 'NONE',  ( 2.864755990943265829, 19.49680007765648071, 2.011557305968487697 ) ) ;
#9145 = EDGE_LOOP ( 'NONE', ( #7400, #7941, #17552, #7669 ) ) ;
#9146 = ADVANCED_FACE ( 'NONE', ( #15932 ), #17711, .F. ) ;
#9147 = CIRCLE ( 'NONE', #1166, 0.1999999999999987899 ) ;
#9148 = AXIS2_PLACEMENT_3D ( 'NONE', #13248, #568, #3526 ) ;
#9149 = CARTESIAN_POINT ( 'NONE',  ( 8.000000000000005329, 36.39999999999999147, 2.499999999999997780 ) ) ;
#9150 = DIRECTION ( 'NONE',  ( -0.000000000000000000, -1.000000000000000000, -0.000000000000000000 ) ) ;
#9151 = CARTESIAN_POINT ( 'NONE',  ( 8.499999999999994671, 13.00000000000000178, 20.49999999999999645 ) ) ;
#9152 = CARTESIAN_POINT ( 'NONE',  ( 6.616872821575479513, -14.16311011709497691, -2.134317094043340024 ) ) ;
#9153 = ADVANCED_BREP_SHAPE_REPRESENTATION ( '', ( #14305, #16940 ), #6566 ) ;
#9154 = DIRECTION ( 'NONE',  ( 0.000000000000000000, -0.5000000000000012212, -0.8660254037844380415 ) ) ;
#9155 = CARTESIAN_POINT ( 'NONE',  ( -2.121784821875005722, -29.93271310232382021, -12.05962931858445231 ) ) ;
#9156 = ORIENTED_EDGE ( 'NONE', *, *, #13115, .F. ) ;
#9157 = LINE ( 'NONE', #13598, #2116 ) ;
#9158 = CARTESIAN_POINT ( 'NONE',  ( -4.000000000000000888, -23.01301540041918869, -8.584512005813342839 ) ) ;
#9159 = ORIENTED_EDGE ( 'NONE', *, *, #150, .T. ) ;
#9160 = ORIENTED_EDGE ( 'NONE', *, *, #8407, .T. ) ;
#9161 = CARTESIAN_POINT ( 'NONE',  ( -4.000000000000004441, -23.27007316922370705, -4.925310638870541879 ) ) ;
#9162 = CARTESIAN_POINT ( 'NONE',  ( 1.533898589781675205E-14, -28.28997139934942950, -9.146999014867043698 ) ) ;
#9163 = VECTOR ( 'NONE', #11369, 1000.000000000000000 ) ;
#9164 = CARTESIAN_POINT ( 'NONE',  ( -4.518350579753602325, 26.87819992234354416, 1.405661355842794391 ) ) ;
#9165 = CARTESIAN_POINT ( 'NONE',  ( 1.027846397803612311, 36.25319992234354771, 3.346150245485499219 ) ) ;
#9166 = CIRCLE ( 'NONE', #1181, 0.9999999999999991118 ) ;
#9167 = CARTESIAN_POINT ( 'NONE',  ( -2.518350579753611207, 16.87819992234354416, 0.7558219633769609480 ) ) ;
#9168 = ORIENTED_EDGE ( 'NONE', *, *, #3663, .F. ) ;
#9169 = CARTESIAN_POINT ( 'NONE',  ( 4.499999999999999112, 19.24680007765647716, -0.05647727720537982360 ) ) ;
#9170 = EDGE_CURVE ( 'NONE', #646, #11774, #7872, .T. ) ;
#9171 = CARTESIAN_POINT ( 'NONE',  ( 4.000000000000000888, -22.30321455972984168, -7.570811349998943562 ) ) ;
#9172 = ORIENTED_EDGE ( 'NONE', *, *, #11507, .F. ) ;
#9173 = DIRECTION ( 'NONE',  ( -1.000000000000000000, 0.000000000000000000, 4.336808689942021680E-16 ) ) ;
#9174 = CARTESIAN_POINT ( 'NONE',  ( -3.481649420246369697, 40.37180007765648071, 1.193696214020542490 ) ) ;
#9175 = CARTESIAN_POINT ( 'NONE',  ( 4.000000000000000888, -25.40052731602546032, -11.99423238915951551 ) ) ;
#9176 = VECTOR ( 'NONE', #4772, 999.9999999999998863 ) ;
#9177 = CARTESIAN_POINT ( 'NONE',  ( 4.243569643750003451, -17.83885414675612324, -5.466534036473456482 ) ) ;
#9178 = CARTESIAN_POINT ( 'NONE',  ( 2.121784821875004390, -20.45966831953192511, -11.34518962918543927 ) ) ;
#9179 = FACE_OUTER_BOUND ( 'NONE', #11891, .T. ) ;
#9180 = VERTEX_POINT ( 'NONE', #11836 ) ;
#9181 = CARTESIAN_POINT ( 'NONE',  ( 4.950315044627312311, -10.00000000000193090, 20.01801554165957953 ) ) ;
#9182 = CARTESIAN_POINT ( 'NONE',  ( -1.734723475976807094E-15, 20.99999999999999289, -2.500000000000000000 ) ) ;
#9183 = DIRECTION ( 'NONE',  ( 1.000000000000000000, 0.000000000000000000, 0.000000000000000000 ) ) ;
#9184 = CARTESIAN_POINT ( 'NONE',  ( -3.999999999999997335, -20.88466450731445079, -9.571229827256534151 ) ) ;
#9185 = ORIENTED_EDGE ( 'NONE', *, *, #1184, .F. ) ;
#9186 = CARTESIAN_POINT ( 'NONE',  ( 2.864755990943222308, 28.00319992234354416, -2.011557305968548093 ) ) ;
#9187 = DIRECTION ( 'NONE',  ( -0.000000000000000000, -1.000000000000000000, -0.000000000000000000 ) ) ;
#9188 = CARTESIAN_POINT ( 'NONE',  ( -2.121784821875005722, -24.77052517516444752, -4.687260919983497587 ) ) ;
#9189 = CARTESIAN_POINT ( 'NONE',  ( -0.05938372350926768989, 21.12180007765648426, -2.628655560595669183 ) ) ;
#9190 = TOROIDAL_SURFACE ( 'NONE', #13633, 9.000000000000001776, 0.9999999999999991118 ) ;
#9191 = CARTESIAN_POINT ( 'NONE',  ( -1.444289557195956863, 16.50319992234354416, 4.262301884875733471 ) ) ;
#9192 = CARTESIAN_POINT ( 'NONE',  ( -4.243569643750000786, -26.22325101726895369, -13.16920360318992955 ) ) ;
#9193 = CARTESIAN_POINT ( 'NONE',  ( 4.713407268011036227E-15, -22.06871753343203579, -15.28855070346190459 ) ) ;
#9194 = CARTESIAN_POINT ( 'NONE',  ( 2.121784821874994176, -23.98544242790896774, -3.566046559362932467 ) ) ;
#9195 = CARTESIAN_POINT ( 'NONE',  ( 2.211161402132902243, 17.12180007765648071, 2.942372952327172442 ) ) ;
#9196 = CARTESIAN_POINT ( 'NONE',  ( 0.000000000000000000, 9.254131787996968228, 30.52396275209373044 ) ) ;
#9197 = EDGE_CURVE ( 'NONE', #17590, #2896, #6187, .T. ) ;
#9198 = CIRCLE ( 'NONE', #13042, 0.9999999999999991118 ) ;
#9199 = CARTESIAN_POINT ( 'NONE',  ( 1.300000000000000044, -0.7216878364870317197, -1.250000000000000000 ) ) ;
#9200 = ADVANCED_FACE ( 'NONE', ( #4886 ), #3724, .T. ) ;
#9201 = FACE_OUTER_BOUND ( 'NONE', #2426, .T. ) ;
#9202 = VERTEX_POINT ( 'NONE', #3503 ) ;
#9203 = ORIENTED_EDGE ( 'NONE', *, *, #17859, .T. ) ;
#9204 =( BOUNDED_CURVE ( )  B_SPLINE_CURVE ( 2, ( #10593, #9019, #7810, #9112, #6240, #10308, #4658, #16085, #7620 ),
 .UNSPECIFIED., .F., .F. ) 
 B_SPLINE_CURVE_WITH_KNOTS ( ( 3, 2, 2, 2, 3 ),
 ( 0.9741379310344827624, 0.9770114942528735913, 0.9827586206896551380, 0.9885057471264367956, 0.9913793103448276245 ),
 .UNSPECIFIED. ) 
 CURVE ( )  GEOMETRIC_REPRESENTATION_ITEM ( )  RATIONAL_B_SPLINE_CURVE ( ( 0.9330127018922194093, 0.9330127018922194093, 1.000000000000000000, 0.8660254037844387076, 1.000000000000000000, 0.8660254037844387076, 1.000000000000000000, 0.9330127018922180770, 0.9330127018922194093 ) ) 
 REPRESENTATION_ITEM ( '' )  );
#9205 = CARTESIAN_POINT ( 'NONE',  ( 0.000000000000000000, 13.00000000000000178, 0.000000000000000000 ) ) ;
#9206 = CARTESIAN_POINT ( 'NONE',  ( 1.999999999999994449, -23.63520233397325399, -3.433610174171729312 ) ) ;
#9207 = LINE ( 'NONE', #12165, #2035 ) ;
#9208 = EDGE_CURVE ( 'NONE', #14942, #156, #14394, .T. ) ;
#9209 = ORIENTED_EDGE ( 'NONE', *, *, #9036, .T. ) ;
#9210 = CARTESIAN_POINT ( 'NONE',  ( 1.497042530366522461, 28.62819992234355126, 2.161531897785029965 ) ) ;
#9211 =( LENGTH_UNIT ( ) NAMED_UNIT ( * ) SI_UNIT ( .MILLI., .METRE. ) );
#9212 = CARTESIAN_POINT ( 'NONE',  ( -4.243569643749997233, -23.94744319389470633, -14.19050330815125704 ) ) ;
#9213 = CARTESIAN_POINT ( 'NONE',  ( -0.05938372350927861171, 23.62180007765647005, -3.680117784833935701 ) ) ;
#9214 = EDGE_CURVE ( 'NONE', #2806, #5635, #17383, .T. ) ;
#9215 = LINE ( 'NONE', #11707, #17622 ) ;
#9216 = CARTESIAN_POINT ( 'NONE',  ( -1.734723475976807094E-15, 16.59999999999999787, -2.500000000000000000 ) ) ;
#9217 = AXIS2_PLACEMENT_3D ( 'NONE', #13180, #15793, #403 ) ;
#9218 = CARTESIAN_POINT ( 'NONE',  ( -2.121784821874996396, -22.99774405038527547, -14.96993742516424497 ) ) ;
#9219 = EDGE_CURVE ( 'NONE', #10898, #17470, #1968, .T. ) ;
#9220 = CARTESIAN_POINT ( 'NONE',  ( 3.064183985264992582, -21.85725672082847382, -2.451266466499125052 ) ) ;
#9221 = CIRCLE ( 'NONE', #1247, 4.000000000000000888 ) ;
#9222 = CARTESIAN_POINT ( 'NONE',  ( -9.000000000000003553, 43.00000000000000000, -2.500000000000001776 ) ) ;
#9223 = CARTESIAN_POINT ( 'NONE',  ( -2.121784821875005722, -25.80296276059631921, -6.161734599703687643 ) ) ;
#9224 = ORIENTED_EDGE ( 'NONE', *, *, #14005, .F. ) ;
#9225 = DIRECTION ( 'NONE',  ( -0.000000000000000000, 1.000000000000000000, -0.000000000000000000 ) ) ;
#9226 = DIRECTION ( 'NONE',  ( 0.000000000000000000, 0.000000000000000000, 1.000000000000000000 ) ) ;
#9227 = CARTESIAN_POINT ( 'NONE',  ( 2.055738996568313048, 31.99680007765648426, 1.423772053676023441 ) ) ;
#9228 = DIRECTION ( 'NONE',  ( 0.000000000000000000, 0.8191520442889952403, -0.5735764363510413855 ) ) ;
#9229 = CARTESIAN_POINT ( 'NONE',  ( 2.798362969681366330, 26.49680007765648071, -2.102939460078824929 ) ) ;
#9230 = FACE_OUTER_BOUND ( 'NONE', #7115, .T. ) ;
#9231 = PRODUCT_CONTEXT ( 'NONE', #16747, 'mechanical' ) ;
#9232 = CARTESIAN_POINT ( 'NONE',  ( -8.000000000000001776, 29.79999999999999716, 2.499999999999995115 ) ) ;
#9233 = EDGE_LOOP ( 'NONE', ( #4091, #17813, #5530, #7043 ) ) ;
#9234 = CIRCLE ( 'NONE', #3030, 0.9999999999999991118 ) ;
#9235 = CARTESIAN_POINT ( 'NONE',  ( -2.121784821875005722, -25.31900764242513091, -5.470575062334849470 ) ) ;
#9236 = CARTESIAN_POINT ( 'NONE',  ( 1.135272562821090458, 19.74680007765648071, 3.311245368580554072 ) ) ;
#9237 = CIRCLE ( 'NONE', #10716, 6.000000000000000000 ) ;
#9238 = ORIENTED_EDGE ( 'NONE', *, *, #14993, .F. ) ;
#9239 = PRODUCT_DEFINITION_FORMATION_WITH_SPECIFIED_SOURCE ( 'ANY', '', #13293, .NOT_KNOWN. ) ;
#9240 = FACE_OUTER_BOUND ( 'NONE', #2400, .T. ) ;
#9241 = CARTESIAN_POINT ( 'NONE',  ( 3.579096709490575479E-14, -22.86967407583208711, -1.406012196336041020 ) ) ;
#9242 = CARTESIAN_POINT ( 'NONE',  ( -3.083685924183309446, -24.92688910118828716, -15.92291992907465747 ) ) ;
#9243 = CARTESIAN_POINT ( 'NONE',  ( 1.999999999999994449, -27.50684327934278528, -8.962886473122447129 ) ) ;
#9244 = CARTESIAN_POINT ( 'NONE',  ( -4.243569643750005227, -22.27216965350720201, -3.254984517416200873 ) ) ;
#9245 = ORIENTED_EDGE ( 'NONE', *, *, #10738, .T. ) ;
#9246 = CARTESIAN_POINT ( 'NONE',  ( 3.579096709490575479E-14, -26.48320562484364871, -6.566670075356708658 ) ) ;
#9247 = AXIS2_PLACEMENT_3D ( 'NONE', #3580, #9045, #11822 ) ;
#9248 = CARTESIAN_POINT ( 'NONE',  ( -1.999999999999996225, -19.70218892076468364, -9.895638628843521190 ) ) ;
#9249 = TOROIDAL_SURFACE ( 'NONE', #4521, 9.000000000000003553, 0.9999999999999991118 ) ;
#9250 = EDGE_LOOP ( 'NONE', ( #3870, #5283 ) ) ;
#9251 = EDGE_LOOP ( 'NONE', ( #8730, #10779, #2252, #3495 ) ) ;
#9252 = CARTESIAN_POINT ( 'NONE',  ( -5.577813053751546416E-15, -24.35380310418546657, -3.525568109927051275 ) ) ;
#9253 = CARTESIAN_POINT ( 'NONE',  ( 3.673772985318163098, 35.50319992234354771, -2.599342558261029001 ) ) ;
#9254 = CARTESIAN_POINT ( 'NONE',  ( -0.05938372350920064630, 33.87819992234354061, 3.680117784833935701 ) ) ;
#9255 = CARTESIAN_POINT ( 'NONE',  ( 1.989345975306457071, 18.50319992234354416, 1.515154207786300500 ) ) ;
#9256 = ORIENTED_EDGE ( 'NONE', *, *, #3538, .T. ) ;
#9257 = CARTESIAN_POINT ( 'NONE',  ( 4.518350579753633411, 19.37180007765647716, 1.405661355842698468 ) ) ;
#9258 = CARTESIAN_POINT ( 'NONE',  ( -2.000000000000005773, -24.19443935941551160, -4.232283417353504440 ) ) ;
#9259 = ORIENTED_EDGE ( 'NONE', *, *, #2542, .T. ) ;
#9260 = VECTOR ( 'NONE', #12214, 1000.000000000000000 ) ;
#9261 = DIRECTION ( 'NONE',  ( -0.000000000000000000, -0.5735764363510414965, -0.8191520442889950182 ) ) ;
#9262 = VECTOR ( 'NONE', #7972, 1000.000000000000000 ) ;
#9263 = CARTESIAN_POINT ( 'NONE',  ( -2.798362969681365886, 35.24680007765648071, 2.102939460078824929 ) ) ;
#9264 = CARTESIAN_POINT ( 'NONE',  ( 10.00000000000000000, 27.59999999999999432, -2.500000000000003109 ) ) ;
#9265 = EDGE_CURVE ( 'NONE', #13163, #7772, #8965, .T. ) ;
#9266 = CARTESIAN_POINT ( 'NONE',  ( 2.121784821874994176, -22.66263177157437525, -1.676877157221437376 ) ) ;
#9267 = CARTESIAN_POINT ( 'NONE',  ( 4.243569643750003451, -22.25897755938633793, -11.77912447777552352 ) ) ;
#9268 = CARTESIAN_POINT ( 'NONE',  ( -4.000000000000000888, -22.94848805062475350, -8.492357399824065567 ) ) ;
#9269 = EDGE_CURVE ( 'NONE', #7853, #18081, #17031, .T. ) ;
#9270 = ORIENTED_EDGE ( 'NONE', *, *, #10062, .F. ) ;
#9271 = CARTESIAN_POINT ( 'NONE',  ( -6.503403972913312181, -10.00000000000000178, 16.98026834952698039 ) ) ;
#9272 = DIRECTION ( 'NONE',  ( 0.000000000000000000, 0.000000000000000000, -1.000000000000000000 ) ) ;
#9273 = PRODUCT_DEFINITION_SHAPE ( 'NONE', 'NONE',  #18381 ) ;
#9274 = FILL_AREA_STYLE_COLOUR ( '', #8937 ) ;
#9275 = CARTESIAN_POINT ( 'NONE',  ( 4.243569643750003451, -25.09818091932399398, -15.83392709700605039 ) ) ;
#9276 = ORIENTED_EDGE ( 'NONE', *, *, #16871, .F. ) ;
#9277 = AXIS2_PLACEMENT_3D ( 'NONE', #9359, #13625, #15309 ) ;
#9278 = CARTESIAN_POINT ( 'NONE',  ( 1.135272562821020070, 27.75319992234354416, -3.311245368580577164 ) ) ;
#9279 = CARTESIAN_POINT ( 'NONE',  ( 8.000000000000001776, 25.39999999999999503, -2.500000000000002220 ) ) ;
#9280 = CARTESIAN_POINT ( 'NONE',  ( 4.730628863548789710E-15, -16.56322023426900714, -7.916230118663721171 ) ) ;
#9281 = CARTESIAN_POINT ( 'NONE',  ( -0.05938372350926768989, 18.62180007765648071, -2.628655560595669183 ) ) ;
#9282 = CARTESIAN_POINT ( 'NONE',  ( -4.499999999999999112, 14.50319992234354594, -0.05647727720528529505 ) ) ;
#9283 = CARTESIAN_POINT ( 'NONE',  ( 4.000000000000003553, -24.51970517198423849, -14.76260590693127028 ) ) ;
#9284 = VERTEX_POINT ( 'NONE', #7075 ) ;
#9285 = CARTESIAN_POINT ( 'NONE',  ( 2.121784821874994176, -23.72733303155099804, -3.197428139432884286 ) ) ;
#9286 = CARTESIAN_POINT ( 'NONE',  ( -0.05938372350927861171, 16.12180007765647716, -3.680117784833935701 ) ) ;
#9287 = AXIS2_PLACEMENT_3D ( 'NONE', #11989, #14799, #6056 ) ;
#9288 = DIRECTION ( 'NONE',  ( 0.000000000000000000, 0.000000000000000000, -1.000000000000000000 ) ) ;
#9289 = CARTESIAN_POINT ( 'NONE',  ( 3.276967058447619152, -25.10900663730464188, -15.57833582608148326 ) ) ;
#9290 = CARTESIAN_POINT ( 'NONE',  ( -1.734723475976807094E-15, 31.99999999999999289, -2.500000000000000000 ) ) ;
#9291 = ORIENTED_EDGE ( 'NONE', *, *, #15618, .F. ) ;
#9292 = ORIENTED_EDGE ( 'NONE', *, *, #12355, .T. ) ;
#9293 = CARTESIAN_POINT ( 'NONE',  ( -3.518350579753630747, 15.62180007765647538, -1.080741659609802729 ) ) ;
#9294 = CARTESIAN_POINT ( 'NONE',  ( 4.000000000000000888, -21.59341372045036778, -6.557110696198077626 ) ) ;
#9295 = CARTESIAN_POINT ( 'NONE',  ( 0.000000000000000000, 3.000000000000000000, -2.499999999999999556 ) ) ;
#9296 = VERTEX_POINT ( 'NONE', #4577 ) ;
#9297 = CARTESIAN_POINT ( 'NONE',  ( 0.05938372350921204690, 27.62819992234354416, -2.628655560595669183 ) ) ;
#9298 = CARTESIAN_POINT ( 'NONE',  ( -5.330712181944245322E-15, -30.14034773130410372, -10.22041724427257137 ) ) ;
#9299 = CARTESIAN_POINT ( 'NONE',  ( 3.518350579753631191, 26.87180007765647360, 1.080741659609802285 ) ) ;
#9300 = PRODUCT_DEFINITION_SHAPE ( 'NONE', 'NONE',  #155 ) ;
#9301 = CYLINDRICAL_SURFACE ( 'NONE', #14030, 0.9999999999999991118 ) ;
#9302 = CARTESIAN_POINT ( 'NONE',  ( 3.108848142585227681, -10.00000000000000178, -11.78746955954679976 ) ) ;
#9303 = EDGE_CURVE ( 'NONE', #2685, #7975, #9645, .T. ) ;
#9304 = CARTESIAN_POINT ( 'NONE',  ( 2.121784821874994176, -28.88952095871037429, -10.56979653803383989 ) ) ;
#9305 = ADVANCED_FACE ( 'NONE', ( #4301 ), #10234, .T. ) ;
#9306 =( BOUNDED_CURVE ( )  B_SPLINE_CURVE ( 2, ( #5733, #8592, #4335, #15750, #11463, #8877, #14357, #6095, #13050 ),
 .UNSPECIFIED., .F., .T. ) 
 B_SPLINE_CURVE_WITH_KNOTS ( ( 3, 2, 2, 2, 3 ),
 ( 0.5431034482758620996, 0.5459770114942529284, 0.5517241379310344751, 0.5574712643678161328, 0.5603448275862069616 ),
 .UNSPECIFIED. ) 
 CURVE ( )  GEOMETRIC_REPRESENTATION_ITEM ( )  RATIONAL_B_SPLINE_CURVE ( ( 0.9330127018922194093, 0.9330127018922194093, 1.000000000000000000, 0.8660254037844387076, 1.000000000000000000, 0.8660254037844387076, 1.000000000000000000, 0.9330127018922180770, 0.9330127018922194093 ) ) 
 REPRESENTATION_ITEM ( '' )  );
#9307 = DIRECTION ( 'NONE',  ( -0.000000000000000000, -0.5735764363510414965, -0.8191520442889950182 ) ) ;
#9308 = CARTESIAN_POINT ( 'NONE',  ( -0.05938372350928957516, 21.12180007765647360, -4.731580009072201776 ) ) ;
#9309 = CARTESIAN_POINT ( 'NONE',  ( 4.299564228933482956E-15, -23.09182937521185863, -15.67085720930136006 ) ) ;
#9310 = LINE ( 'NONE', #10979, #14452 ) ;
#9311 = CARTESIAN_POINT ( 'NONE',  ( 4.243569643749996345, -25.76740106252136542, -8.246692287302257895 ) ) ;
#9312 = B_SPLINE_CURVE_WITH_KNOTS ( 'NONE', 3,
 ( #11873, #5012, #673, #6499, #5100, #14868 ),
 .UNSPECIFIED., .F., .F.,
 ( 4, 2, 4 ),
 ( 0.000000000000000000, 0.001225725630168212092, 0.002451451260336424184 ),
 .UNSPECIFIED. ) ;
#9313 = ORIENTED_EDGE ( 'NONE', *, *, #548, .T. ) ;
#9314 = CARTESIAN_POINT ( 'NONE',  ( 0.000000000000000000, 18.79999999999999361, 2.500000000000000000 ) ) ;
#9315 = LINE ( 'NONE', #12000, #17477 ) ;
#9316 = CARTESIAN_POINT ( 'NONE',  ( -0.8262555684461330152, 33.49680007765648071, -2.360188852285403982 ) ) ;
#9317 = VERTEX_POINT ( 'NONE', #15620 ) ;
#9318 = CARTESIAN_POINT ( 'NONE',  ( -1.135272562821090014, 33.49680007765648071, -3.311245368580554072 ) ) ;
#9319 = CARTESIAN_POINT ( 'NONE',  ( -8.000000000000003553, 23.19999999999999574, -2.500000000000001776 ) ) ;
#9320 = FACE_OUTER_BOUND ( 'NONE', #3514, .T. ) ;
#9321 = EDGE_CURVE ( 'NONE', #15889, #11926, #2565, .T. ) ;
#9322 = EDGE_CURVE ( 'NONE', #6383, #8354, #9936, .T. ) ;
#9323 = EDGE_LOOP ( 'NONE', ( #14934, #7531, #14245, #16646 ) ) ;
#9324 = CARTESIAN_POINT ( 'NONE',  ( -4.243569643750000786, -22.09350067554145625, -7.271308884309165776 ) ) ;
#9325 = CARTESIAN_POINT ( 'NONE',  ( 1.027846397803542144, 23.74680007765647716, -3.346150245485522312 ) ) ;
#9326 = EDGE_CURVE ( 'NONE', #12622, #10092, #12899, .T. ) ;
#9327 = ORIENTED_EDGE ( 'NONE', *, *, #16722, .T. ) ;
#9328 =( NAMED_UNIT ( * ) SI_UNIT ( $, .STERADIAN. ) SOLID_ANGLE_UNIT ( ) );
#9329 = CARTESIAN_POINT ( 'NONE',  ( -0.3167908498167790188, -23.77648345714862543, -16.77767476633956534 ) ) ;
#9330 = CARTESIAN_POINT ( 'NONE',  ( 1.300000000000000044, -1.082531754730548190, 0.6250000000000002220 ) ) ;
#9331 = CARTESIAN_POINT ( 'NONE',  ( -1.071796769724505882, -17.66000535097569113, -7.913408556114437609 ) ) ;
#9332 = CARTESIAN_POINT ( 'NONE',  ( -4.243569643750000786, -19.77051610831973605, -3.953743104938735708 ) ) ;
#9333 = ORIENTED_EDGE ( 'NONE', *, *, #2834, .T. ) ;
#9334 = DIRECTION ( 'NONE',  ( 3.469446951953612217E-16, -0.000000000000000000, 1.000000000000000000 ) ) ;
#9335 = CARTESIAN_POINT ( 'NONE',  ( -5.279047395330986450E-15, -27.50631746662347155, -6.948976581196172120 ) ) ;
#9336 = CARTESIAN_POINT ( 'NONE',  ( 3.481649420246369697, 29.12180007765647005, -1.193696214020541824 ) ) ;
#9337 = ORIENTED_EDGE ( 'NONE', *, *, #2769, .F. ) ;
#9338 = ORIENTED_EDGE ( 'NONE', *, *, #16261, .T. ) ;
#9339 = CARTESIAN_POINT ( 'NONE',  ( -4.000000000000003553, 6.938893903907228378E-15, 0.000000000000000000 ) ) ;
#9340 = CARTESIAN_POINT ( 'NONE',  ( 4.499999999999999112, 35.75319992234354061, 0.05647727720528474687 ) ) ;
#9341 = CARTESIAN_POINT ( 'NONE',  ( 3.481649420246395010, 33.37819992234354061, 1.193696214020467439 ) ) ;
#9342 = CARTESIAN_POINT ( 'NONE',  ( -2.481649420246391902, 24.62819992234354416, -0.8687765177875723666 ) ) ;
#9343 = ORIENTED_EDGE ( 'NONE', *, *, #1627, .T. ) ;
#9344 = CARTESIAN_POINT ( 'NONE',  ( 4.499999999999999112, 21.74680007765647360, -0.05647727720537982360 ) ) ;
#9345 = AXIS2_PLACEMENT_3D ( 'NONE', #1561, #2782, #3045 ) ;
#9346 = CARTESIAN_POINT ( 'NONE',  ( 4.713407268011036227E-15, -16.90652960627266310, -7.916182304860950758 ) ) ;
#9347 = VERTEX_POINT ( 'NONE', #8554 ) ;
#9348 = CARTESIAN_POINT ( 'NONE',  ( -1.071796769724496334, -24.88154859762023463, -4.279266784443063187 ) ) ;
#9349 = CARTESIAN_POINT ( 'NONE',  ( -2.798362969681365886, 40.24680007765648071, 2.102939460078824929 ) ) ;
#9350 = LINE ( 'NONE', #9264, #17315 ) ;
#9351 = ADVANCED_FACE ( 'NONE', ( #14323 ), #8837, .F. ) ;
#9352 = CARTESIAN_POINT ( 'NONE',  ( 3.250762944584260072, -21.87258937905581746, -2.200190645090608133 ) ) ;
#9353 = AXIS2_PLACEMENT_3D ( 'NONE', #5410, #2465, #6883 ) ;
#9354 = CARTESIAN_POINT ( 'NONE',  ( -2.121784821874996396, -21.19097827587949467, -12.38960848565391260 ) ) ;
#9355 = CARTESIAN_POINT ( 'NONE',  ( 4.898587196589413815E-16, 2.700915433685006750, 35.11257424290206330 ) ) ;
#9356 = ORIENTED_EDGE ( 'NONE', *, *, #4113, .T. ) ;
#9357 = AXIS2_PLACEMENT_3D ( 'NONE', #356, #13041, #7287 ) ;
#9358 = CARTESIAN_POINT ( 'NONE',  ( -6.681132651088828034, -10.00000000000000178, 19.92483346546715950 ) ) ;
#9359 = CARTESIAN_POINT ( 'NONE',  ( -1.734723475976807094E-15, 43.00000000000000000, -2.500000000000000000 ) ) ;
#9360 = CARTESIAN_POINT ( 'NONE',  ( -3.999999999999997335, -20.82013715752001559, -9.479075221267256879 ) ) ;
#9361 = CARTESIAN_POINT ( 'NONE',  ( -5.330712181944245322E-15, -30.68883019856478711, -11.00373138662392236 ) ) ;
#9362 = EDGE_LOOP ( 'NONE', ( #4873, #325, #8241, #14764 ) ) ;
#9363 = CARTESIAN_POINT ( 'NONE',  ( -2.211161402132839182, 39.12819992234354771, 2.942372952327218627 ) ) ;
#9364 = CARTESIAN_POINT ( 'NONE',  ( 0.05938372350920110426, 15.12819992234354416, -3.680117784833935701 ) ) ;
#9365 = CARTESIAN_POINT ( 'NONE',  ( 4.243569643750003451, -17.83885414675612324, -5.466534036473456482 ) ) ;
#9366 = CARTESIAN_POINT ( 'NONE',  ( -1.497042530366477164, 27.62180007765648426, 2.161531897785062384 ) ) ;
#9367 = CARTESIAN_POINT ( 'NONE',  ( 3.607379964056363075, 18.50319992234354416, 2.690724712371229010 ) ) ;
#9368 = CARTESIAN_POINT ( 'NONE',  ( 4.000000000000000888, -25.40052731602546032, -11.99423238915951551 ) ) ;
#9369 = ORIENTED_EDGE ( 'NONE', *, *, #16096, .F. ) ;
#9370 = ADVANCED_FACE ( 'NONE', ( #1533, #7167 ), #17311, .T. ) ;
#9371 = CARTESIAN_POINT ( 'NONE',  ( -2.121784821874996396, -17.06122793415199723, -6.491713766773147931 ) ) ;
#9372 = AXIS2_PLACEMENT_3D ( 'NONE', #2577, #15277, #2669 ) ;
#9373 = CARTESIAN_POINT ( 'NONE',  ( -2.733110507866247652, 40.12180007765647360, 3.862833514489154574 ) ) ;
#9374 = EDGE_CURVE ( 'NONE', #15136, #7792, #44, .T. ) ;
#9375 = DIRECTION ( 'NONE',  ( -1.000000000000000000, 0.000000000000000000, 4.336808689942021680E-16 ) ) ;
#9376 = DIRECTION ( 'NONE',  ( -0.000000000000000000, 1.000000000000000000, -0.000000000000000000 ) ) ;
#9377 = FACE_OUTER_BOUND ( 'NONE', #12136, .T. ) ;
#9378 = VERTEX_POINT ( 'NONE', #4395 ) ;
#9379 = ORIENTED_EDGE ( 'NONE', *, *, #8794, .F. ) ;
#9380 = CARTESIAN_POINT ( 'NONE',  ( -8.500000000000005329, 13.00000000000000000, -18.35000000000000142 ) ) ;
#9381 = CARTESIAN_POINT ( 'NONE',  ( -1.734723475976807094E-15, 43.00000000000000000, -12.50000000000000000 ) ) ;
#9382 = CARTESIAN_POINT ( 'NONE',  ( -5.577813053751546416E-15, -26.41867827504920996, -6.474515469367432274 ) ) ;
#9383 = EDGE_LOOP ( 'NONE', ( #15399, #8960, #10380, #15109 ) ) ;
#9384 = CARTESIAN_POINT ( 'NONE',  ( 0.8262555684460829442, 35.25319992234354771, -2.360188852285421302 ) ) ;
#9385 = VECTOR ( 'NONE', #7889, 1000.000000000000000 ) ;
#9386 = CARTESIAN_POINT ( 'NONE',  ( 4.243569643750003451, -21.71049509212565454, -10.99581033542417252 ) ) ;
#9387 = CARTESIAN_POINT ( 'NONE',  ( -3.500000000000000444, 22.99680007765647716, 0.05647727720536892260 ) ) ;
#9388 = FACE_OUTER_BOUND ( 'NONE', #15084, .T. ) ;
#9389 = CARTESIAN_POINT ( 'NONE',  ( 4.730628863548789710E-15, -21.75767183597312737, -15.33467581975593141 ) ) ;
#9390 = ADVANCED_FACE ( 'NONE', ( #10035 ), #3196, .F. ) ;
#9391 = AXIS2_PLACEMENT_3D ( 'NONE', #4252, #14076, #3978 ) ;
#9392 = VECTOR ( 'NONE', #53, 1000.000000000000000 ) ;
#9393 = CARTESIAN_POINT ( 'NONE',  ( 3.878940541574451562, -25.96705729343073443, -15.31857466066475304 ) ) ;
#9394 = CARTESIAN_POINT ( 'NONE',  ( 3.673772985318219053, 24.49680007765648071, 2.599342558260951730 ) ) ;
#9395 = CARTESIAN_POINT ( 'NONE',  ( -4.000000000000004441, -28.17415170002511360, -11.92906061754144886 ) ) ;
#9396 = CARTESIAN_POINT ( 'NONE',  ( 8.500000000000001776, 15.00000000000000178, -18.35000000000000142 ) ) ;
#9397 = CARTESIAN_POINT ( 'NONE',  ( 2.121784821874994176, -24.72750694243812219, -4.625824516661818819 ) ) ;
#9398 = ORIENTED_EDGE ( 'NONE', *, *, #12816, .T. ) ;
#9399 = CYLINDRICAL_SURFACE ( 'NONE', #14866, 4.000000000000000000 ) ;
#9400 = DIRECTION ( 'NONE',  ( -0.000000000000000000, -1.000000000000000000, -0.000000000000000000 ) ) ;
#9401 = CARTESIAN_POINT ( 'NONE',  ( -1.989345975306426206, 30.24680007765648426, 1.515154207786343799 ) ) ;
#9402 = DIRECTION ( 'NONE',  ( 0.000000000000000000, 0.8191520442889952403, -0.5735764363510413855 ) ) ;
#9403 = CARTESIAN_POINT ( 'NONE',  ( -3.500000000000000444, 27.99680007765648071, 0.05647727720536892260 ) ) ;
#9404 = CLOSED_SHELL ( 'NONE', ( #8559, #3207, #13458, #13654, #12218, #9200, #10895, #4112, #15161, #1287 ) ) ;
#9405 = CARTESIAN_POINT ( 'NONE',  ( 9.000000000000001776, 25.39999999999999503, -2.500000000000002665 ) ) ;
#9406 = MECHANICAL_DESIGN_GEOMETRIC_PRESENTATION_REPRESENTATION (  '', ( #15052 ), #11484 ) ;
#9407 = DIRECTION ( 'NONE',  ( 0.000000000000000000, -1.000000000000000000, 0.000000000000000000 ) ) ;
#9408 = AXIS2_PLACEMENT_3D ( 'NONE', #12635, #8373, #18324 ) ;
#9409 = EDGE_LOOP ( 'NONE', ( #6958, #11642, #17188, #11419 ) ) ;
#9410 = CARTESIAN_POINT ( 'NONE',  ( 4.243569643750003451, -18.90355540673274248, -6.987085018684902948 ) ) ;
#9411 = CARTESIAN_POINT ( 'NONE',  ( -2.115076519116362519, 27.62180007765648071, 3.012182706137107147 ) ) ;
#9412 =( BOUNDED_CURVE ( )  B_SPLINE_CURVE ( 2, ( #16221, #10545, #3515, #5076, #740, #9161, #2136, #6197, #11847 ),
 .UNSPECIFIED., .F., .T. ) 
 B_SPLINE_CURVE_WITH_KNOTS ( ( 3, 2, 2, 2, 3 ),
 ( 0.7672413793103448620, 0.7701149425287355799, 0.7758620689655172376, 0.7816091954022988952, 0.7844827586206897241 ),
 .UNSPECIFIED. ) 
 CURVE ( )  GEOMETRIC_REPRESENTATION_ITEM ( )  RATIONAL_B_SPLINE_CURVE ( ( 0.9330127018922194093, 0.9330127018922206306, 1.000000000000000000, 0.8660254037844387076, 1.000000000000000000, 0.8660254037844387076, 1.000000000000000000, 0.9330127018922180770, 0.9330127018922194093 ) ) 
 REPRESENTATION_ITEM ( '' )  );
#9413 = ORIENTED_EDGE ( 'NONE', *, *, #8011, .F. ) ;
#9414 = CARTESIAN_POINT ( 'NONE',  ( 3.579096709490575479E-14, -25.12813129325936501, -4.631423369717193594 ) ) ;
#9415 = FACE_OUTER_BOUND ( 'NONE', #14730, .T. ) ;
#9416 = CARTESIAN_POINT ( 'NONE',  ( -1.734723475976807094E-15, 36.39999999999999147, -11.50000000000000178 ) ) ;
#9417=STYLED_ITEM('',(#18396),#14659);
#9418 = CARTESIAN_POINT ( 'NONE',  ( 9.566593547379630635, -9.974457738288718289, -0.6241947029430978677 ) ) ;
#9420 = CARTESIAN_POINT ( 'NONE',  ( -4.000000000000000888, -20.88361287976100300, -5.543410040383684567 ) ) ;
#9419 = CIRCLE ( 'NONE', #8525, 0.9999999999999991118 ) ;
#9421 = CARTESIAN_POINT ( 'NONE',  ( -4.243569643749997233, -24.46366198661064573, -14.92774014801135074 ) ) ;
#9422 = ADVANCED_FACE ( 'NONE', ( #3011 ), #12010, .F. ) ;
#9423 = ORIENTED_EDGE ( 'NONE', *, *, #7099, .F. ) ;
#9424 = CARTESIAN_POINT ( 'NONE',  ( -5.279047395330986450E-15, -25.95766108847566400, -4.737266061615885704 ) ) ;
#9425 = CARTESIAN_POINT ( 'NONE',  ( -3.500000000000000444, 30.49680007765647716, 0.05647727720536892260 ) ) ;
#9426 = EDGE_CURVE ( 'NONE', #17255, #18179, #1257, .T. ) ;
#9427 = ORIENTED_EDGE ( 'NONE', *, *, #10897, .F. ) ;
#9428 = ORIENTED_EDGE ( 'NONE', *, *, #15229, .T. ) ;
#9429 = CARTESIAN_POINT ( 'NONE',  ( -4.000000000000002665, 2.343145750507625191, 2.343145750507618086 ) ) ;
#9430 = EDGE_CURVE ( 'NONE', #8069, #2307, #14610, .T. ) ;
#9431 = CARTESIAN_POINT ( 'NONE',  ( -0.05938372350918959958, 33.87819992234354061, 4.731580009072201776 ) ) ;
#9432 = FACE_OUTER_BOUND ( 'NONE', #18157, .T. ) ;
#9433 = CARTESIAN_POINT ( 'NONE',  ( -2.518350579753611207, 26.87819992234354416, 0.7558219633769609480 ) ) ;
#9434 = ORIENTED_EDGE ( 'NONE', *, *, #11755, .F. ) ;
#9435 = ADVANCED_FACE ( 'NONE', ( #16279 ), #1972, .T. ) ;
#9436 = CIRCLE ( 'NONE', #5603, 8.000000000000003553 ) ;
#9437 = CARTESIAN_POINT ( 'NONE',  ( -2.829195390882805139, 25.87180007765647716, -3.793023760679206102 ) ) ;
#9438 = CARTESIAN_POINT ( 'NONE',  ( 3.999999999999996447, -22.40970851469715441, -3.696582572437044245 ) ) ;
#9439 = ORIENTED_EDGE ( 'NONE', *, *, #8967, .F. ) ;
#9440 = DIRECTION ( 'NONE',  ( -0.000000000000000000, -0.5000000000000001110, 0.8660254037844385966 ) ) ;
#9441 = CARTESIAN_POINT ( 'NONE',  ( 3.518350579753631191, 39.37180007765646650, 1.080741659609802285 ) ) ;
#9442 = EDGE_CURVE ( 'NONE', #3449, #4032, #3150, .T. ) ;
#9443 = CARTESIAN_POINT ( 'NONE',  ( 2.200000000000000178, 0.000000000000000000, 0.000000000000000000 ) ) ;
#9444 = CARTESIAN_POINT ( 'NONE',  ( 2.121784821875004390, -17.58820128504952152, -7.244309707463659542 ) ) ;
#9445 = CIRCLE ( 'NONE', #1160, 8.000000000000001776 ) ;
#9446 =( BOUNDED_CURVE ( )  B_SPLINE_CURVE ( 2, ( #8175, #18133, #10867, #5309, #12164, #7897, #17854, #16644, #1146 ),
 .UNSPECIFIED., .F., .F. ) 
 B_SPLINE_CURVE_WITH_KNOTS ( ( 3, 2, 2, 2, 3 ),
 ( 0.02586206896551724796, 0.02873563218390804558, 0.03448275862068965469, 0.04022988505747126381, 0.04310344827586207184 ),
 .UNSPECIFIED. ) 
 CURVE ( )  GEOMETRIC_REPRESENTATION_ITEM ( )  RATIONAL_B_SPLINE_CURVE ( ( 0.9330127018922194093, 0.9330127018922195203, 1.000000000000000000, 0.8660254037844387076, 1.000000000000000000, 0.8660254037844387076, 1.000000000000000000, 0.9330127018922192983, 0.9330127018922194093 ) ) 
 REPRESENTATION_ITEM ( '' )  );
#9447 = CARTESIAN_POINT ( 'NONE',  ( -4.243569643750005227, -26.14381059887672976, -8.784260816366916913 ) ) ;
#9448 = PRODUCT ( 'armature', 'armature', '', ( #17794 ) ) ;
#9449 = AXIS2_PLACEMENT_3D ( 'NONE', #12587, #16792, #16972 ) ;
#9450 = CARTESIAN_POINT ( 'NONE',  ( -1.734723475976807094E-15, 38.59999999999999432, -2.500000000000000000 ) ) ;
#9451 = ORIENTED_EDGE ( 'NONE', *, *, #9269, .T. ) ;
#9452 = CARTESIAN_POINT ( 'NONE',  ( -3.706921591972381904E-14, -18.44586024076842534, -9.035725650560502586 ) ) ;
#9453 = CARTESIAN_POINT ( 'NONE',  ( 1.135272562821090458, 17.24680007765647716, 3.311245368580554072 ) ) ;
#9454 = CARTESIAN_POINT ( 'NONE',  ( 2.000000000000004441, -19.22898836077508022, -9.219838192305099156 ) ) ;
#9455 = ORIENTED_EDGE ( 'NONE', *, *, #9321, .T. ) ;
#9456 = CARTESIAN_POINT ( 'NONE',  ( -1.027846397803611866, 32.50319992234354771, -3.346150245485499219 ) ) ;
#9457 = CARTESIAN_POINT ( 'NONE',  ( -0.05938372350920064630, 16.37819992234354416, 3.680117784833935701 ) ) ;
#9458 = CARTESIAN_POINT ( 'NONE',  ( -5.330712181944245322E-15, -23.68761282235488963, -1.004956746021377967 ) ) ;
#9459 = CARTESIAN_POINT ( 'NONE',  ( -2.500000000000001332, 32.99680007765648071, 0.05647727720535858364 ) ) ;
#9460 = CARTESIAN_POINT ( 'NONE',  ( 1.444289557195957086, 22.75319992234354061, -4.262301884875733471 ) ) ;
#9461 = CIRCLE ( 'NONE', #283, 3.799999999999999378 ) ;
#9462 = CARTESIAN_POINT ( 'NONE',  ( 1.999999999999994449, -27.24873388298481558, -8.594268053192397616 ) ) ;
#9463 = ORIENTED_EDGE ( 'NONE', *, *, #6248, .T. ) ;
#9464 = AXIS2_PLACEMENT_3D ( 'NONE', #9687, #3861, #5616 ) ;
#9465 = DIRECTION ( 'NONE',  ( 1.000000000000000000, 0.000000000000000000, 0.000000000000000000 ) ) ;
#9466 = CARTESIAN_POINT ( 'NONE',  ( 4.518350579753633411, 36.87180007765647360, 1.405661355842698468 ) ) ;
#9467 = CARTESIAN_POINT ( 'NONE',  ( -4.243569643749998122, -21.88256802303095938, -11.24155594871087338 ) ) ;
#9468 = CARTESIAN_POINT ( 'NONE',  ( -4.000000000000003553, 6.938893903907228378E-15, 0.000000000000000000 ) ) ;
#9469 = DIRECTION ( 'NONE',  ( -1.000000000000000000, 0.000000000000000000, 4.336808689942021680E-16 ) ) ;
#9470 = VERTEX_POINT ( 'NONE', #5040 ) ;
#9471 = ORIENTED_EDGE ( 'NONE', *, *, #4450, .F. ) ;
#9472 = CARTESIAN_POINT ( 'NONE',  ( -1.734723475976807094E-15, 40.79999999999999716, -2.500000000000000000 ) ) ;
#9473 = CARTESIAN_POINT ( 'NONE',  ( 8.000000000000000000, 0.000000000000000000, 0.000000000000000000 ) ) ;
#9474 = LINE ( 'NONE', #6517, #13263 ) ;
#9475 = ORIENTED_EDGE ( 'NONE', *, *, #10152, .T. ) ;
#9476 = CIRCLE ( 'NONE', #5627, 2.149999999999995470 ) ;
#9477 = CARTESIAN_POINT ( 'NONE',  ( 1.135272562821020070, 15.25319992234354594, -3.311245368580577164 ) ) ;
#9478 = CARTESIAN_POINT ( 'NONE',  ( -2.121784821875005722, -26.57729094967022831, -7.267589859493831739 ) ) ;
#9479 = CARTESIAN_POINT ( 'NONE',  ( -2.115076519116362519, 30.12180007765647360, 3.012182706137107147 ) ) ;
#9480 = CARTESIAN_POINT ( 'NONE',  ( 3.500000000000000444, 28.25319992234354416, 0.05647727720529520379 ) ) ;
#9481 = CARTESIAN_POINT ( 'NONE',  ( 8.500000000000001776, 15.00000000000000178, -18.35000000000000142 ) ) ;
#9482 = CARTESIAN_POINT ( 'NONE',  ( 1.533898589781675205E-14, -28.48355344591296401, -9.423462828807814162 ) ) ;
#9483 = CARTESIAN_POINT ( 'NONE',  ( -5.330712181944245322E-15, -28.10773623498509721, -7.317547187323446778 ) ) ;
#9484 = VECTOR ( 'NONE', #6955, 1000.000000000000227 ) ;
#9485 = CARTESIAN_POINT ( 'NONE',  ( 4.150834101209824212, -27.15734369766470380, -14.50322620280942587 ) ) ;
#9486 = CARTESIAN_POINT ( 'NONE',  ( 2.733110507866247652, 21.37180007765647360, -3.862833514489153686 ) ) ;
#9487 = CYLINDRICAL_SURFACE ( 'NONE', #3840, 0.9999999999999991118 ) ;
#9488 = DIRECTION ( 'NONE',  ( -3.469446951953613696E-16, -0.000000000000000000, -1.000000000000000000 ) ) ;
#9489 = CARTESIAN_POINT ( 'NONE',  ( -4.243569643750000786, -22.31934639735467840, -7.593850001747957990 ) ) ;
#9490 = ORIENTED_EDGE ( 'NONE', *, *, #11512, .F. ) ;
#9491 = CARTESIAN_POINT ( 'NONE',  ( -2.000000000000005773, -29.61473668293285399, -11.97327023588450601 ) ) ;
#9492 = FACE_OUTER_BOUND ( 'NONE', #3799, .T. ) ;
#9493 = CARTESIAN_POINT ( 'NONE',  ( -2.518350579753628526, 38.12180007765647360, -0.7558219633769075463 ) ) ;
#9494 = ADVANCED_FACE ( 'NONE', ( #7818 ), #5508, .T. ) ;
#9495 = CARTESIAN_POINT ( 'NONE',  ( 1.071796769724485454, -20.07057066942950385, -11.35605261078598360 ) ) ;
#9496 = CARTESIAN_POINT ( 'NONE',  ( -3.518350579753630303, 38.12180007765647360, -1.080741659609802952 ) ) ;
#9497 = DIRECTION ( 'NONE',  ( 3.469446951953612217E-16, -0.000000000000000000, 1.000000000000000000 ) ) ;
#9498 = ITEM_DEFINED_TRANSFORMATION ( 'NONE', 'NONE', #4496,  #16940 ) ;
#9499 = AXIS2_PLACEMENT_3D ( 'NONE', #14335, #7270, #12926 ) ;
#9500 = DIRECTION ( 'NONE',  ( 1.000000000000000000, 0.000000000000000000, -4.336808689942021680E-16 ) ) ;
#9501 = ORIENTED_EDGE ( 'NONE', *, *, #3203, .F. ) ;
#9502 = CARTESIAN_POINT ( 'NONE',  ( -5.330712181944246111E-15, -25.78475166776338057, -3.999981407953017598 ) ) ;
#9503 = CARTESIAN_POINT ( 'NONE',  ( -2.798362969681365886, 22.74680007765648071, 2.102939460078824929 ) ) ;
#9504 = ORIENTED_EDGE ( 'NONE', *, *, #684, .F. ) ;
#9505 = DIRECTION ( 'NONE',  ( 0.000000000000000000, 0.8191520442889952403, -0.5735764363510413855 ) ) ;
#9506 = CARTESIAN_POINT ( 'NONE',  ( -4.243569643750000786, -26.70720613544014199, -13.86036314055876772 ) ) ;
#9507 = CARTESIAN_POINT ( 'NONE',  ( -8.500000000000005329, 13.00000000000000178, -20.49999999999999645 ) ) ;
#9508 = CIRCLE ( 'NONE', #16049, 4.324969328314200112 ) ;
#9509 = CARTESIAN_POINT ( 'NONE',  ( -4.000000000000000888, -22.43226925790881765, -7.755120559963970983 ) ) ;
#9510 = CARTESIAN_POINT ( 'NONE',  ( 0.000000000000000000, 33.00000000000000000, 6.000000000000000888 ) ) ;
#9511 = CARTESIAN_POINT ( 'NONE',  ( -4.243569643750000786, -26.70720613544014199, -13.86036314055876772 ) ) ;
#9512 = VERTEX_POINT ( 'NONE', #14827 ) ;
#9513 = LINE ( 'NONE', #3688, #8311 ) ;
#9514 = CARTESIAN_POINT ( 'NONE',  ( 4.000000000000003553, -19.42204459461930099, -7.482392114319591947 ) ) ;
#9515 = CARTESIAN_POINT ( 'NONE',  ( 2.864755990943265829, 39.49680007765647360, 2.011557305968487697 ) ) ;
#9516 = ORIENTED_EDGE ( 'NONE', *, *, #1070, .F. ) ;
#9517 = VERTEX_POINT ( 'NONE', #8027 ) ;
#9518 = CARTESIAN_POINT ( 'NONE',  ( 1.999999999999994449, -25.24838606191550028, -5.737475299741293888 ) ) ;
#9519 = FILL_AREA_STYLE ('',( #3055 ) ) ;
#9520 = CARTESIAN_POINT ( 'NONE',  ( 2.829195390882724759, 37.87819992234353350, -3.793023760679264278 ) ) ;
#9521 = UNCERTAINTY_MEASURE_WITH_UNIT (LENGTH_MEASURE( 1.000000000000000082E-05 ), #13827, 'distance_accuracy_value', 'NONE');
#9522 = CARTESIAN_POINT ( 'NONE',  ( -1.661723472263481630E-14, -20.25262601527420969, -11.61605459007084029 ) ) ;
#9523 = CARTESIAN_POINT ( 'NONE',  ( -2.500000000000001332, 29.50319992234354771, -0.05647727720530596601 ) ) ;
#9524 =( BOUNDED_CURVE ( )  B_SPLINE_CURVE ( 2, ( #7744, #14816, #2114, #12004, #17699, #2293, #6717, #8200, #6538 ),
 .UNSPECIFIED., .F., .T. ) 
 B_SPLINE_CURVE_WITH_KNOTS ( ( 3, 2, 2, 2, 3 ),
 ( 0.04310344827586207184, 0.04597701149425287293, 0.05172413793103448204, 0.05747126436781609116, 0.06034482758620690612 ),
 .UNSPECIFIED. ) 
 CURVE ( )  GEOMETRIC_REPRESENTATION_ITEM ( )  RATIONAL_B_SPLINE_CURVE ( ( 0.9330127018922194093, 0.9330127018922194093, 1.000000000000000000, 0.8660254037844387076, 1.000000000000000000, 0.8660254037844387076, 1.000000000000000000, 0.9330127018922191873, 0.9330127018922194093 ) ) 
 REPRESENTATION_ITEM ( '' )  );
#9525 = ORIENTED_EDGE ( 'NONE', *, *, #4447, .F. ) ;
#9526 = CARTESIAN_POINT ( 'NONE',  ( -2.121784821875005722, -28.93253919143669251, -10.63123294135551689 ) ) ;
#9527 = CARTESIAN_POINT ( 'NONE',  ( -3.673772985318219053, 23.24680007765647716, -2.599342558260952174 ) ) ;
#9528 = UNCERTAINTY_MEASURE_WITH_UNIT (LENGTH_MEASURE( 1.000000000000000082E-05 ), #1465, 'distance_accuracy_value', 'NONE');
#9529 = CARTESIAN_POINT ( 'NONE',  ( -2.000000000000005773, -23.93632996305754190, -3.863664997423455816 ) ) ;
#9530 = ORIENTED_EDGE ( 'NONE', *, *, #2661, .T. ) ;
#9531 = EDGE_CURVE ( 'NONE', #9655, #14197, #3160, .T. ) ;
#9532 = DIRECTION ( 'NONE',  ( 0.000000000000000000, 0.000000000000000000, 1.000000000000000000 ) ) ;
#9533 = CARTESIAN_POINT ( 'NONE',  ( 8.000000000000000000, 5.388445916248356971E-16, 4.400000000000002132 ) ) ;
#9534 = AXIS2_PLACEMENT_3D ( 'NONE', #4615, #12864, #14360 ) ;
#9535 = CARTESIAN_POINT ( 'NONE',  ( -4.243569643749998122, -18.01092707766142809, -5.712279649760158229 ) ) ;
#9536 = PRESENTATION_LAYER_ASSIGNMENT (  '', '', ( #17571 ) ) ;
#9537 = CARTESIAN_POINT ( 'NONE',  ( -4.243569643750000786, -23.12593826097332794, -8.745782564029356720 ) ) ;
#9538 = PRODUCT_DEFINITION_FORMATION_WITH_SPECIFIED_SOURCE ( 'ANY', '', #6486, .NOT_KNOWN. ) ;
#9539 = DIRECTION ( 'NONE',  ( 0.000000000000000000, 1.000000000000000000, 0.000000000000000000 ) ) ;
#9540 = ORIENTED_EDGE ( 'NONE', *, *, #8794, .T. ) ;
#9541 = CARTESIAN_POINT ( 'NONE',  ( -4.000000000000000888, -24.56167177856700334, -10.79622252539362925 ) ) ;
#9542 = CARTESIAN_POINT ( 'NONE',  ( 1.071796769724494780, -28.47202674519411758, -9.407000994151900386 ) ) ;
#9543 = CARTESIAN_POINT ( 'NONE',  ( -0.05938372350927861865, 16.12180007765647716, -3.680117784833935701 ) ) ;
#9544 = ORIENTED_EDGE ( 'NONE', *, *, #755, .T. ) ;
#9545 = CARTESIAN_POINT ( 'NONE',  ( 2.798362969681409851, 33.50319992234354771, 2.102939460078764977 ) ) ;
#9546 = CARTESIAN_POINT ( 'NONE',  ( 2.115076519116425580, 23.62819992234354061, 3.012182706137062294 ) ) ;
#9547 = CARTESIAN_POINT ( 'NONE',  ( 2.121784821874994176, -23.69506935700625050, -3.151350836941627875 ) ) ;
#9548 = CARTESIAN_POINT ( 'NONE',  ( 0.7188294034286049072, 28.74680007765648426, -2.395093729190366005 ) ) ;
#9549 = AXIS2_PLACEMENT_3D ( 'NONE', #12300, #18261, #16409 ) ;
#9550 = CARTESIAN_POINT ( 'NONE',  ( -2.829195390882724315, 29.12819992234354416, 3.793023760679264722 ) ) ;
#9551 = UNCERTAINTY_MEASURE_WITH_UNIT (LENGTH_MEASURE( 1.000000000000000082E-05 ), #12168, 'distance_accuracy_value', 'NONE');
#9552 = CARTESIAN_POINT ( 'NONE',  ( 4.000000000000003553, -22.71293939747845769, -12.18227696742093791 ) ) ;
#9553 = ORIENTED_EDGE ( 'NONE', *, *, #15, .T. ) ;
#9554 = ADVANCED_FACE ( 'NONE', ( #17887 ), #14099, .F. ) ;
#9555 = CARTESIAN_POINT ( 'NONE',  ( 4.243569643750003451, -18.12922721765884049, -5.881229758894760629 ) ) ;
#9556 = EDGE_CURVE ( 'NONE', #7574, #456, #13414, .T. ) ;
#9557 = AXIS2_PLACEMENT_3D ( 'NONE', #13134, #16028, #8961 ) ;
#9558 = CARTESIAN_POINT ( 'NONE',  ( -2.798362969681365886, 25.24680007765647716, 2.102939460078824929 ) ) ;
#9559 = CARTESIAN_POINT ( 'NONE',  ( -2.000000000000005773, -27.09817006914760640, -8.379240642573305919 ) ) ;
#9560 = CARTESIAN_POINT ( 'NONE',  ( -2.121784821875005722, -26.83540034602819802, -7.636208279423879475 ) ) ;
#9561 = CARTESIAN_POINT ( 'NONE',  ( 4.000000000000003553, -24.26159577562626524, -14.39398748700122077 ) ) ;
#9562 = VECTOR ( 'NONE', #1014, 1000.000000000000227 ) ;
#9563 = CARTESIAN_POINT ( 'NONE',  ( -5.577813053751546416E-15, -26.22509622848567545, -6.198051655426662698 ) ) ;
#9564 = VECTOR ( 'NONE', #10938, 1000.000000000000114 ) ;
#9565 = CARTESIAN_POINT ( 'NONE',  ( 9.000000000000005329, -10.00000000000000000, 30.00000000000000000 ) ) ;
#9566 = ORIENTED_EDGE ( 'NONE', *, *, #4447, .T. ) ;
#9567 = EDGE_LOOP ( 'NONE', ( #11004, #16157, #11698, #11865 ) ) ;
#9568 = CARTESIAN_POINT ( 'NONE',  ( 1.135272562821090458, 17.24680007765647716, 3.311245368580554072 ) ) ;
#9569 = DIRECTION ( 'NONE',  ( 0.000000000000000000, 0.000000000000000000, -1.000000000000000000 ) ) ;
#9570 = CARTESIAN_POINT ( 'NONE',  ( -1.734723475976807094E-15, 25.39999999999999503, -2.500000000000000000 ) ) ;
#9571 = ORIENTED_EDGE ( 'NONE', *, *, #6035, .F. ) ;
#9572 = CARTESIAN_POINT ( 'NONE',  ( 0.7188294034286553114, 36.25319992234354771, 2.395093729190349130 ) ) ;
#9573 = CARTESIAN_POINT ( 'NONE',  ( -5.330712181944245322E-15, -28.84980074951425877, -8.377325144622332687 ) ) ;
#9574 = CARTESIAN_POINT ( 'NONE',  ( -2.115076519116362519, 27.62180007765648071, 3.012182706137107147 ) ) ;
#9575 = CARTESIAN_POINT ( 'NONE',  ( 0.05938372350920109732, 25.12819992234354416, -3.680117784833935701 ) ) ;
#9576 = DIRECTION ( 'NONE',  ( -1.000000000000000000, -0.000000000000000000, -0.000000000000000000 ) ) ;
#9577 = CARTESIAN_POINT ( 'NONE',  ( -1.734723475976807094E-15, 40.79999999999999716, -2.500000000000000000 ) ) ;
#9578 = AXIS2_PLACEMENT_3D ( 'NONE', #2388, #16758, #13953 ) ;
#9579 = CARTESIAN_POINT ( 'NONE',  ( 2.121784821875004390, -20.71777771588989125, -11.71380804911548701 ) ) ;
#9580 = DIRECTION ( 'NONE',  ( -1.000000000000000000, 0.000000000000000000, 4.336808689942021680E-16 ) ) ;
#9581 = CARTESIAN_POINT ( 'NONE',  ( 2.733110507866247652, 23.87180007765647716, -3.862833514489153686 ) ) ;
#9582 = CARTESIAN_POINT ( 'NONE',  ( -4.648177544792955347E-16, -29.58051838113927090, -10.99009111451728415 ) ) ;
#9583 = FACE_OUTER_BOUND ( 'NONE', #5717, .T. ) ;
#9584 = CARTESIAN_POINT ( 'NONE',  ( -5.330712181944245322E-15, -25.75248799321863657, -3.953904105461760743 ) ) ;
#9585 = AXIS2_PLACEMENT_3D ( 'NONE', #17778, #1153, #16741 ) ;
#9586 = DIRECTION ( 'NONE',  ( -1.000000000000000000, -0.000000000000000000, -0.000000000000000000 ) ) ;
#9587 = DIRECTION ( 'NONE',  ( -0.000000000000000000, 1.000000000000000000, -0.000000000000000000 ) ) ;
#9588 = CARTESIAN_POINT ( 'NONE',  ( -2.500000000000001332, 35.49680007765647360, 0.05647727720535858364 ) ) ;
#9589 = AXIS2_PLACEMENT_3D ( 'NONE', #9443, #13896, #8142 ) ;
#9590 = DIRECTION ( 'NONE',  ( -1.000000000000000000, 0.000000000000000000, 4.336808689942021680E-16 ) ) ;
#9591 = CARTESIAN_POINT ( 'NONE',  ( -0.05938372350927861865, 38.62180007765647360, -3.680117784833935701 ) ) ;
#9592 = AXIS2_PLACEMENT_3D ( 'NONE', #15906, #7635, #1918 ) ;
#9593 = LINE ( 'NONE', #13670, #5713 ) ;
#9594 = ADVANCED_FACE ( 'NONE', ( #1090 ), #5250, .F. ) ;
#9595 = CARTESIAN_POINT ( 'NONE',  ( -1.860401164264412488, 15.00000000000001243, -3.294166817225182786 ) ) ;
#9596 = ORIENTED_EDGE ( 'NONE', *, *, #18354, .T. ) ;
#9597 = CARTESIAN_POINT ( 'NONE',  ( 2.121784821874994176, -25.01788001334084299, -5.040520239083123855 ) ) ;
#9598 = EDGE_CURVE ( 'NONE', #6179, #7574, #17398, .T. ) ;
#9599 = CARTESIAN_POINT ( 'NONE',  ( -3.518350579753630747, 28.12180007765647360, -1.080741659609802729 ) ) ;
#9600 = EDGE_CURVE ( 'NONE', #17010, #15166, #16797, .T. ) ;
#9601 = AXIS2_PLACEMENT_3D ( 'NONE', #13350, #14948, #7781 ) ;
#9602 = CARTESIAN_POINT ( 'NONE',  ( 2.000000000000004441, -18.90635161462267178, -8.759065166385774148 ) ) ;
#9603 = EDGE_CURVE ( 'NONE', #9076, #4809, #7888, .T. ) ;
#9604 = DIRECTION ( 'NONE',  ( 0.000000000000000000, 0.000000000000000000, -1.000000000000000000 ) ) ;
#9605 = DIRECTION ( 'NONE',  ( 0.000000000000000000, 0.000000000000000000, -1.000000000000000000 ) ) ;
#9606 = DIRECTION ( 'NONE',  ( 3.469446951953612217E-16, -0.000000000000000000, 1.000000000000000000 ) ) ;
#9607 = DIRECTION ( 'NONE',  ( 0.000000000000000000, 0.000000000000000000, 1.000000000000000000 ) ) ;
#9608 = CARTESIAN_POINT ( 'NONE',  ( 2.121784821875004390, -23.52471740128279620, -15.72253336585475658 ) ) ;
#9609 = VERTEX_POINT ( 'NONE', #12290 ) ;
#9610 = CARTESIAN_POINT ( 'NONE',  ( -14.99999999999999645, -10.00000000000000000, 30.00000000000000000 ) ) ;
#9611 = CARTESIAN_POINT ( 'NONE',  ( -1.999999999999996225, -19.18597012804874069, -9.158401788983423941 ) ) ;
#9612 = CARTESIAN_POINT ( 'NONE',  ( 3.500000000000000444, 39.24680007765647360, -0.05647727720536935281 ) ) ;
#9613 = ORIENTED_EDGE ( 'NONE', *, *, #3658, .F. ) ;
#9614 = CARTESIAN_POINT ( 'NONE',  ( -5.577813053751546416E-15, -24.35380310418546657, -3.525568109927051275 ) ) ;
#9615 = CARTESIAN_POINT ( 'NONE',  ( 4.518350579753602325, 38.12819992234354061, -1.405661355842793725 ) ) ;
#9616 = DIRECTION ( 'NONE',  ( 0.000000000000000000, 0.000000000000000000, 1.000000000000000000 ) ) ;
#9617 = CARTESIAN_POINT ( 'NONE',  ( -0.8262555684460826111, 24.00319992234354416, 2.360188852285421302 ) ) ;
#9618 = ORIENTED_EDGE ( 'NONE', *, *, #9800, .T. ) ;
#9619 = CARTESIAN_POINT ( 'NONE',  ( -4.243569643750004339, -27.95057637338251411, -11.36458975587725106 ) ) ;
#9620 = CARTESIAN_POINT ( 'NONE',  ( 2.829195390882805583, 27.12180007765647716, 3.793023760679204770 ) ) ;
#9621 = CARTESIAN_POINT ( 'NONE',  ( 4.713407268011036227E-15, -16.39031081355672725, -7.178945465000852622 ) ) ;
#9622 = EDGE_LOOP ( 'NONE', ( #10639, #4327 ) ) ;
#9623 = PLANE ( 'NONE',  #879 ) ;
#9624 = FACE_OUTER_BOUND ( 'NONE', #12758, .T. ) ;
#9625 = DIRECTION ( 'NONE',  ( -0.000000000000000000, 1.000000000000000000, -0.000000000000000000 ) ) ;
#9626 = CARTESIAN_POINT ( 'NONE',  ( 4.730628863548789710E-15, -18.91846847603547133, -11.27987320052540809 ) ) ;
#9627 = VERTEX_POINT ( 'NONE', #2490 ) ;
#9628 = CARTESIAN_POINT ( 'NONE',  ( -2.908121172428787649, -29.32336267363790938, -12.73959420715949875 ) ) ;
#9629 = ORIENTED_EDGE ( 'NONE', *, *, #18253, .F. ) ;
#9630 = CARTESIAN_POINT ( 'NONE',  ( -5.279047395330986450E-15, -28.28064565569737709, -8.054831840986315328 ) ) ;
#9631 = LINE ( 'NONE', #12230, #3656 ) ;
#9632 = LINE ( 'NONE', #2609, #17857 ) ;
#9633 = ORIENTED_EDGE ( 'NONE', *, *, #9909, .T. ) ;
#9634 = CARTESIAN_POINT ( 'NONE',  ( -0.05938372350920063936, 36.37819992234355482, 3.680117784833935701 ) ) ;
#9635 = CARTESIAN_POINT ( 'NONE',  ( 1.135272562821020070, 20.25319992234354416, -3.311245368580577164 ) ) ;
#9636 = CARTESIAN_POINT ( 'NONE',  ( -4.243569643749997233, -18.01092707766142809, -5.712279649760157341 ) ) ;
#9637 = CARTESIAN_POINT ( 'NONE',  ( 0.7188294034286049072, 33.74680007765648071, -2.395093729190366005 ) ) ;
#9638 = EDGE_CURVE ( 'NONE', #10649, #18210, #2855, .T. ) ;
#9639 = CARTESIAN_POINT ( 'NONE',  ( -3.607379964056363075, 22.25319992234354416, -2.690724712371229899 ) ) ;
#9640 = CARTESIAN_POINT ( 'NONE',  ( 4.713407268011036227E-15, -20.77817055164219084, -13.44545860381166413 ) ) ;
#9641 = ORIENTED_EDGE ( 'NONE', *, *, #7106, .F. ) ;
#9642 = CARTESIAN_POINT ( 'NONE',  ( -4.243569643750000786, -19.77051610831973605, -3.953743104938735708 ) ) ;
#9643 = CARTESIAN_POINT ( 'NONE',  ( -3.518350579753630747, 18.12180007765648071, -1.080741659609802729 ) ) ;
#9644 = CARTESIAN_POINT ( 'NONE',  ( 4.730628863548789710E-15, -18.88620480149072023, -11.23379589803414902 ) ) ;
#9645 = CIRCLE ( 'NONE', #15576, 0.9999999999999991118 ) ;
#9646 = CARTESIAN_POINT ( 'NONE',  ( 4.299564228933482956E-15, -23.15635672500629738, -15.76301181529063733 ) ) ;
#9647 = PLANE ( 'NONE',  #1208 ) ;
#9648 = DIRECTION ( 'NONE',  ( -0.000000000000000000, -1.000000000000000000, -0.000000000000000000 ) ) ;
#9649 = VERTEX_POINT ( 'NONE', #12652 ) ;
#9650 = ORIENTED_EDGE ( 'NONE', *, *, #14664, .F. ) ;
#9651 = DIRECTION ( 'NONE',  ( -0.000000000000000000, -1.000000000000000000, -0.000000000000000000 ) ) ;
#9652 = ADVANCED_FACE ( 'NONE', ( #1452 ), #18278, .T. ) ;
#9653 = CARTESIAN_POINT ( 'NONE',  ( 9.000000000000001776, 16.59999999999999787, -2.500000000000002665 ) ) ;
#9654 = CYLINDRICAL_SURFACE ( 'NONE', #2343, 4.000000000000000000 ) ;
#9655 = VERTEX_POINT ( 'NONE', #4307 ) ;
#9656 = CARTESIAN_POINT ( 'NONE',  ( -1.497042530366522461, 37.37819992234354771, -2.161531897785030409 ) ) ;
#9657 = ADVANCED_FACE ( 'NONE', ( #12564 ), #10840, .T. ) ;
#9658 = CARTESIAN_POINT ( 'NONE',  ( 4.243569643749996345, -26.54172925159527452, -9.352547547092401103 ) ) ;
#9659 = CARTESIAN_POINT ( 'NONE',  ( -2.115076519116362519, 32.62180007765646650, 3.012182706137107147 ) ) ;
#9660 = EDGE_CURVE ( 'NONE', #12347, #11426, #15020, .T. ) ;
#9661 = CARTESIAN_POINT ( 'NONE',  ( -3.481649420246394122, 27.12819992234354771, -1.193696214020467883 ) ) ;
#9662 = LINE ( 'NONE', #13939, #1307 ) ;
#9663 = AXIS2_PLACEMENT_3D ( 'NONE', #518, #4770, #10423 ) ;
#9664 = DIRECTION ( 'NONE',  ( -0.000000000000000000, 1.000000000000000000, -0.000000000000000000 ) ) ;
#9665 = ADVANCED_FACE ( 'NONE', ( #9782 ), #6907, .T. ) ;
#9666 = CARTESIAN_POINT ( 'NONE',  ( -2.121784821875005722, -27.12577341693091171, -8.050904001845182734 ) ) ;
#9667 = CARTESIAN_POINT ( 'NONE',  ( -1.794514420735399352, -10.00000000000000178, -12.33839425357257902 ) ) ;
#9668 = CARTESIAN_POINT ( 'NONE',  ( -4.000000000000004441, -22.56027232994424025, -3.911609985069677276 ) ) ;
#9669 = DIRECTION ( 'NONE',  ( 0.000000000000000000, -1.000000000000000000, 0.000000000000000000 ) ) ;
#9670 = CIRCLE ( 'NONE', #1696, 0.1999999999999987899 ) ;
#9671 = CARTESIAN_POINT ( 'NONE',  ( -4.243569643750005227, -23.53045296075229942, -5.051999314575184030 ) ) ;
#9672 = CARTESIAN_POINT ( 'NONE',  ( -4.000000000000004441, -23.85081931173408165, -5.754702084719914623 ) ) ;
#9673 = PRESENTATION_STYLE_ASSIGNMENT (( #14315 ) ) ;
#9674 = CARTESIAN_POINT ( 'NONE',  ( 2.500000000000001332, 36.74680007765648071, -0.05647727720535888202 ) ) ;
#9675 = CARTESIAN_POINT ( 'NONE',  ( -8.000000000000001776, 38.59999999999999432, 2.499999999999995115 ) ) ;
#9676 = CARTESIAN_POINT ( 'NONE',  ( 2.211161402132902243, 34.62180007765648071, 2.942372952327172442 ) ) ;
#9677 = CARTESIAN_POINT ( 'NONE',  ( -4.000000000000000888, -25.27147261784647014, -11.80992317919449519 ) ) ;
#9678 = CARTESIAN_POINT ( 'NONE',  ( -8.000000000000001776, 29.79999999999999716, 2.499999999999998224 ) ) ;
#9679 = VERTEX_POINT ( 'NONE', #5522 ) ;
#9680 = CARTESIAN_POINT ( 'NONE',  ( -4.243569643750000786, -21.83539127918348299, -6.902690464379118040 ) ) ;
#9681 = CARTESIAN_POINT ( 'NONE',  ( -1.135272562821090014, 20.99680007765647716, -3.311245368580554072 ) ) ;
#9682 = AXIS2_PLACEMENT_3D ( 'NONE', #6667, #8415, #8242 ) ;
#9683 = CIRCLE ( 'NONE', #16528, 8.000000000000001776 ) ;
#9684 = LINE ( 'NONE', #8651, #3883 ) ;
#9685 = CARTESIAN_POINT ( 'NONE',  ( 4.730628863548789710E-15, -22.49973635050228538, -16.39445377705482088 ) ) ;
#9686 = LINE ( 'NONE', #4135, #13515 ) ;
#9687 = CARTESIAN_POINT ( 'NONE',  ( 9.000000000000000000, 38.59999999999999432, -2.500000000000001332 ) ) ;
#9688 = DIRECTION ( 'NONE',  ( -1.000000000000000000, 0.000000000000000000, 0.000000000000000000 ) ) ;
#9689 = CARTESIAN_POINT ( 'NONE',  ( -2.121784821874996396, -22.70737097948255823, -14.55524170274294171 ) ) ;
#9690 = VERTEX_POINT ( 'NONE', #2757 ) ;
#9691 = CARTESIAN_POINT ( 'NONE',  ( 0.000000000000000000, 43.00000000000000000, 0.000000000000000000 ) ) ;
#9692 = CARTESIAN_POINT ( 'NONE',  ( 1.999999999999994449, -24.99027666555753413, -5.368856879811245264 ) ) ;
#9693=STYLED_ITEM('',(#18396),#13807);
#9694 = CARTESIAN_POINT ( 'NONE',  ( -2.211161402132902243, 35.87180007765648782, -2.942372952327172886 ) ) ;
#9695 = AXIS2_PLACEMENT_3D ( 'NONE', #7549, #16104, #13203 ) ;
#9696 = ORIENTED_EDGE ( 'NONE', *, *, #10179, .T. ) ;
#9697 = CARTESIAN_POINT ( 'NONE',  ( -2.829195390882805139, 15.87180007765647716, -3.793023760679206102 ) ) ;
#9698 = UNCERTAINTY_MEASURE_WITH_UNIT (LENGTH_MEASURE( 1.000000000000000082E-05 ), #9720, 'distance_accuracy_value', 'NONE');
#9699 = CARTESIAN_POINT ( 'NONE',  ( -5.577813053751546416E-15, -23.57947491511155036, -2.419712850136908511 ) ) ;
#9700 = CARTESIAN_POINT ( 'NONE',  ( 0.05938372350921204690, 25.12819992234354416, -2.628655560595669183 ) ) ;
#9701 = EDGE_CURVE ( 'NONE', #9017, #14942, #186, .T. ) ;
#9702 = ORIENTED_EDGE ( 'NONE', *, *, #13621, .T. ) ;
#9703 = CARTESIAN_POINT ( 'NONE',  ( -4.243569643749998122, -23.20537867936554832, -13.13072535085236936 ) ) ;
#9704 = CARTESIAN_POINT ( 'NONE',  ( -2.829195390882805139, 28.37180007765647716, -3.793023760679206102 ) ) ;
#9705 = CARTESIAN_POINT ( 'NONE',  ( 4.000000000000003553, -18.06697026303502085, -5.547145408680076883 ) ) ;
#9706 = ORIENTED_EDGE ( 'NONE', *, *, #15424, .T. ) ;
#9707 =( GEOMETRIC_REPRESENTATION_CONTEXT ( 3 ) GLOBAL_UNCERTAINTY_ASSIGNED_CONTEXT ( ( #18086 ) ) GLOBAL_UNIT_ASSIGNED_CONTEXT ( ( #109, #5670, #11053 ) ) REPRESENTATION_CONTEXT ( 'NONE', 'WORKASPACE' ) );
#9708 = CARTESIAN_POINT ( 'NONE',  ( -5.577813053751546416E-15, -24.87002189690140241, -4.262804949787145858 ) ) ;
#9709 = AXIS2_PLACEMENT_3D ( 'NONE', #17301, #3184, #11790 ) ;
#9710 = SURFACE_SIDE_STYLE ('',( #18366 ) ) ;
#9711 = PLANE ( 'NONE',  #14913 ) ;
#9712 = CARTESIAN_POINT ( 'NONE',  ( 1.300000000000000044, -0.7216878364870317197, -1.250000000000000000 ) ) ;
#9713 = CARTESIAN_POINT ( 'NONE',  ( -2.121784821875005722, -25.57711703878310061, -5.839193482264897206 ) ) ;
#9714 = EDGE_LOOP ( 'NONE', ( #10157, #4849, #9833, #442 ) ) ;
#9715 = CARTESIAN_POINT ( 'NONE',  ( 0.000000000000000000, 23.19999999999999574, 2.500000000000000000 ) ) ;
#9716 = ORIENTED_EDGE ( 'NONE', *, *, #660, .T. ) ;
#9717 = CARTESIAN_POINT ( 'NONE',  ( 3.999999999999996447, -26.86209560257706030, -10.05525031723713347 ) ) ;
#9718 = CARTESIAN_POINT ( 'NONE',  ( 1.999999999999994449, -28.02306207205872113, -9.700123312982540824 ) ) ;
#9719 = CARTESIAN_POINT ( 'NONE',  ( -0.05938372350927861865, 23.62180007765647360, -3.680117784833935701 ) ) ;
#9720 =( LENGTH_UNIT ( ) NAMED_UNIT ( * ) SI_UNIT ( .MILLI., .METRE. ) );
#9721 = ORIENTED_EDGE ( 'NONE', *, *, #5518, .F. ) ;
#9722 = SURFACE_STYLE_FILL_AREA ( #15662 ) ;
#9723 = AXIS2_PLACEMENT_3D ( 'NONE', #2420, #4823, #10471 ) ;
#9724 = CARTESIAN_POINT ( 'NONE',  ( -2.864755990943222308, 31.75319992234354416, 2.011557305968548093 ) ) ;
#9725 = CARTESIAN_POINT ( 'NONE',  ( 3.518350579753606322, 20.62819992234354416, -1.080741659609876892 ) ) ;
#9727 = EDGE_CURVE ( 'NONE', #17654, #6273, #6103, .T. ) ;
#9726 = AXIS2_PLACEMENT_3D ( 'NONE', #10182, #15859, #4267 ) ;
#9728 = CARTESIAN_POINT ( 'NONE',  ( 1.999999999999994449, -28.34569881821112602, -10.16089633890186761 ) ) ;
#9729 = CARTESIAN_POINT ( 'NONE',  ( -2.481649420246374138, 27.87180007765648426, 0.8687765177876256573 ) ) ;
#9730 = CARTESIAN_POINT ( 'NONE',  ( -4.481649420246396787, 29.62819992234354416, -1.518615910253363399 ) ) ;
#9731 = UNCERTAINTY_MEASURE_WITH_UNIT (LENGTH_MEASURE( 1.000000000000000082E-05 ), #7022, 'distance_accuracy_value', 'NONE');
#9732 = CARTESIAN_POINT ( 'NONE',  ( 2.000000000000004441, -22.26177376727626367, -13.55110462547639472 ) ) ;
#9733 = ORIENTED_EDGE ( 'NONE', *, *, #8620, .T. ) ;
#9734 = CARTESIAN_POINT ( 'NONE',  ( -2.121784821875005722, -22.99602307520341427, -2.153009282964420290 ) ) ;
#9735 = CARTESIAN_POINT ( 'NONE',  ( -2.798362969681365886, 22.74680007765648071, 2.102939460078824929 ) ) ;
#9736 =( NAMED_UNIT ( * ) SI_UNIT ( $, .STERADIAN. ) SOLID_ANGLE_UNIT ( ) );
#9737 = VECTOR ( 'NONE', #13895, 1000.000000000000000 ) ;
#9738 = CARTESIAN_POINT ( 'NONE',  ( -4.243569643750004339, -24.82099994254214081, -6.895091414225420934 ) ) ;
#9739 = AXIS2_PLACEMENT_3D ( 'NONE', #1964, #3345, #15957 ) ;
#9740 = CARTESIAN_POINT ( 'NONE',  ( 3.999999999999996447, -26.28134946006668926, -9.225858871387760729 ) ) ;
#9741 = DIRECTION ( 'NONE',  ( -1.000000000000000000, 0.000000000000000000, 0.000000000000000000 ) ) ;
#9742 = CARTESIAN_POINT ( 'NONE',  ( -1.661723472263481630E-14, -20.05904396871067874, -11.33959077613006450 ) ) ;
#9743 = VERTEX_POINT ( 'NONE', #12749 ) ;
#9744 = ORIENTED_EDGE ( 'NONE', *, *, #13683, .T. ) ;
#9745 = CARTESIAN_POINT ( 'NONE',  ( 2.798362969681366330, 21.49680007765647716, -2.102939460078824929 ) ) ;
#9746 = DIRECTION ( 'NONE',  ( 1.000000000000000000, 0.000000000000000000, -4.336808689942021680E-16 ) ) ;
#9747 = CARTESIAN_POINT ( 'NONE',  ( -4.000000000000000888, -24.49714442877256459, -10.70406791940435198 ) ) ;
#9748 = DIRECTION ( 'NONE',  ( 0.000000000000000000, 0.8191520442889952403, -0.5735764363510413855 ) ) ;
#9749 = ORIENTED_EDGE ( 'NONE', *, *, #2592, .F. ) ;
#9750 = CARTESIAN_POINT ( 'NONE',  ( 2.481649420246391902, 33.37819992234354771, 0.8687765177875720335 ) ) ;
#9751 = AXIS2_PLACEMENT_3D ( 'NONE', #7552, #4871, #11818 ) ;
#9752 = CARTESIAN_POINT ( 'NONE',  ( 2.121784821875004390, -19.91118585227123816, -10.56187548683408828 ) ) ;
#9753 = CARTESIAN_POINT ( 'NONE',  ( -2.798362969681365886, 30.24680007765648071, 2.102939460078824929 ) ) ;
#9754 = AXIS2_PLACEMENT_3D ( 'NONE', #4227, #2578, #13779 ) ;
#9755 = CARTESIAN_POINT ( 'NONE',  ( 2.211161402132839626, 30.37819992234354416, -2.942372952327218183 ) ) ;
#9756 = CARTESIAN_POINT ( 'NONE',  ( -4.000000000000000888, -21.20624962591340790, -6.004183066303009575 ) ) ;
#9757 = FACE_OUTER_BOUND ( 'NONE', #7854, .T. ) ;
#9758 = CARTESIAN_POINT ( 'NONE',  ( -4.243569643749997233, -21.39861290485977463, -10.55039641134203521 ) ) ;
#9759 = ADVANCED_FACE ( 'NONE', ( #1359 ), #10249, .T. ) ;
#9760 = ADVANCED_FACE ( 'NONE', ( #11433 ), #15586, .F. ) ;
#9761 = CARTESIAN_POINT ( 'NONE',  ( 1.071796769724493670, -23.68410221844107610, -16.51671048980665191 ) ) ;
#9762 = EDGE_CURVE ( 'NONE', #13448, #11075, #2840, .T. ) ;
#9763 = VECTOR ( 'NONE', #5134, 1000.000000000000000 ) ;
#9764 = FACE_OUTER_BOUND ( 'NONE', #6241, .T. ) ;
#9765 = CARTESIAN_POINT ( 'NONE',  ( 4.299564228933482956E-15, -19.28471577963676964, -10.23373551633992129 ) ) ;
#9766 = CARTESIAN_POINT ( 'NONE',  ( 4.243569643749996345, -23.70252589165761492, -5.297744927861876896 ) ) ;
#9767 = DIRECTION ( 'NONE',  ( 0.000000000000000000, 0.000000000000000000, 1.000000000000000000 ) ) ;
#9768 = FACE_OUTER_BOUND ( 'NONE', #4553, .T. ) ;
#9769 = ADVANCED_FACE ( 'NONE', ( #6990 ), #16947, .F. ) ;
#9770 = CARTESIAN_POINT ( 'NONE',  ( -2.481649420246374138, 40.37180007765647360, 0.8687765177876256573 ) ) ;
#9771 = DIRECTION ( 'NONE',  ( -3.469446951953613696E-16, -0.000000000000000000, -1.000000000000000000 ) ) ;
#9772 = CARTESIAN_POINT ( 'NONE',  ( -2.115076519116362519, 40.12180007765648071, 3.012182706137108035 ) ) ;
#9773 = LINE ( 'NONE', #10389, #2175 ) ;
#9774 = ITEM_DEFINED_TRANSFORMATION ( 'NONE', 'NONE', #7160,  #16940 ) ;
#9775 = CARTESIAN_POINT ( 'NONE',  ( 3.064181913176682759, -21.66367673124435100, -2.174801284911689336 ) ) ;
#9776 = ORIENTED_EDGE ( 'NONE', *, *, #1453, .T. ) ;
#9777 = CARTESIAN_POINT ( 'NONE',  ( 4.243569643750003451, -19.93599299216462128, -8.461558698405095669 ) ) ;
#9778 = CONICAL_SURFACE ( 'NONE', #11255, 3.047499999999999876, 1.047197551196590748 ) ;
#9779 = CARTESIAN_POINT ( 'NONE',  ( 2.798362969681366330, 28.99680007765647716, -2.102939460078824929 ) ) ;
#9780 = DIRECTION ( 'NONE',  ( -1.000000000000000000, 0.000000000000000000, 4.336808689942021680E-16 ) ) ;
#9781 = DIRECTION ( 'NONE',  ( -0.000000000000000000, 1.000000000000000000, -0.000000000000000000 ) ) ;
#9782 = FACE_OUTER_BOUND ( 'NONE', #15243, .T. ) ;
#9783 = CARTESIAN_POINT ( 'NONE',  ( 3.082316921986471225, -29.06618978543598786, -12.78463801463987437 ) ) ;
#9784 = CARTESIAN_POINT ( 'NONE',  ( 4.243569643749996345, -28.60660442245902146, -12.30149490653278121 ) ) ;
#9785 = ORIENTED_EDGE ( 'NONE', *, *, #1895, .F. ) ;
#9786 = DIRECTION ( 'NONE',  ( 0.000000000000000000, 0.000000000000000000, -1.000000000000000000 ) ) ;
#9787 = CARTESIAN_POINT ( 'NONE',  ( 4.713407268011036227E-15, -18.00349454149897355, -9.482810590570412757 ) ) ;
#9788 = VECTOR ( 'NONE', #17632, 1000.000000000000000 ) ;
#9789 = CARTESIAN_POINT ( 'NONE',  ( 2.500000000000001332, 16.74680007765648071, -0.05647727720535888202 ) ) ;
#9790 = VERTEX_POINT ( 'NONE', #16766 ) ;
#9791 =( BOUNDED_CURVE ( )  B_SPLINE_CURVE ( 2, ( #8521, #6093, #4272, #14194, #2039, #7662, #7040, #1497, #12704 ),
 .UNSPECIFIED., .F., .T. ) 
 B_SPLINE_CURVE_WITH_KNOTS ( ( 3, 2, 2, 2, 3 ),
 ( 0.9396551724137931494, 0.9425287356321838672, 0.9482758620689655249, 0.9540229885057470716, 0.9568965517241379004 ),
 .UNSPECIFIED. ) 
 CURVE ( )  GEOMETRIC_REPRESENTATION_ITEM ( )  RATIONAL_B_SPLINE_CURVE ( ( 0.9330127018922194093, 0.9330127018922206306, 1.000000000000000000, 0.8660254037844387076, 1.000000000000000000, 0.8660254037844387076, 1.000000000000000000, 0.9330127018922194093, 0.9330127018922194093 ) ) 
 REPRESENTATION_ITEM ( '' )  );
#9792 = CARTESIAN_POINT ( 'NONE',  ( -1.999999999999996225, -19.44407952440671039, -9.527020208913473454 ) ) ;
#9793 = PRESENTATION_STYLE_ASSIGNMENT (( #4319 ) ) ;
#9794 = CARTESIAN_POINT ( 'NONE',  ( 2.733110507866328920, 38.62819992234354771, 3.862833514489095510 ) ) ;
#9795 = DIRECTION ( 'NONE',  ( -1.000000000000000000, -0.000000000000000000, -0.000000000000000000 ) ) ;
#9796 = CARTESIAN_POINT ( 'NONE',  ( -2.500000000000001332, 32.00319992234354061, -0.05647727720530596601 ) ) ;
#9797 = EDGE_LOOP ( 'NONE', ( #7403, #18348, #7015, #1479 ) ) ;
#9798 = CARTESIAN_POINT ( 'NONE',  ( -4.243569643750004339, -26.91813878795063530, -9.890116076157061897 ) ) ;
#9799 = CARTESIAN_POINT ( 'NONE',  ( -1.336863392178478716, 29.99680007765647716, 4.297206761780677731 ) ) ;
#9800 = EDGE_CURVE ( 'NONE', #9856, #6744, #9686, .T. ) ;
#9801 = VERTEX_POINT ( 'NONE', #15369 ) ;
#9802 = CARTESIAN_POINT ( 'NONE',  ( 0.000000000000000000, 5.977523610840987267, 32.81826849749789687 ) ) ;
#9803 = LINE ( 'NONE', #18097, #9737 ) ;
#9804 = CARTESIAN_POINT ( 'NONE',  ( 9.000000000000005329, -10.00000000000000000, 30.00000000000000000 ) ) ;
#9805 = DIRECTION ( 'NONE',  ( -1.000000000000000000, 0.000000000000000000, -0.000000000000000000 ) ) ;
#9806 = CARTESIAN_POINT ( 'NONE',  ( 2.121784821875004390, -19.16912133774208016, -9.502097529535200593 ) ) ;
#9807 = ORIENTED_EDGE ( 'NONE', *, *, #15615, .F. ) ;
#9808 = CARTESIAN_POINT ( 'NONE',  ( 1.300000000000000044, 0.7216878364870329410, -1.250000000000000000 ) ) ;
#9809 = ORIENTED_EDGE ( 'NONE', *, *, #12833, .F. ) ;
#9810 = CARTESIAN_POINT ( 'NONE',  ( 4.713407268011036227E-15, -20.58458850507865989, -13.16899478987089189 ) ) ;
#9811 = DIRECTION ( 'NONE',  ( -1.000000000000000000, 0.000000000000000000, 4.336808689942021680E-16 ) ) ;
#9812 = DIRECTION ( 'NONE',  ( 0.000000000000000000, 1.000000000000000000, 0.000000000000000000 ) ) ;
#9813 = CARTESIAN_POINT ( 'NONE',  ( -3.500000000000000444, 39.50319992234354771, -0.05647727720529563400 ) ) ;
#9814 = CARTESIAN_POINT ( 'NONE',  ( 1.027846397803612311, 21.25319992234354416, 3.346150245485499219 ) ) ;
#9815 = CARTESIAN_POINT ( 'NONE',  ( -2.000000000000005773, -28.38871705093744779, -10.22233274222354460 ) ) ;
#9816 = CARTESIAN_POINT ( 'NONE',  ( 0.8262555684461332373, 34.74680007765647360, 2.360188852285403982 ) ) ;
#9817 = CARTESIAN_POINT ( 'NONE',  ( 4.481649420246397675, 23.37819992234354416, 1.518615910253363177 ) ) ;
#9818 = CARTESIAN_POINT ( 'NONE',  ( 4.713407268011036227E-15, -19.74573296621031915, -11.97098492409147319 ) ) ;
#9819 = EDGE_LOOP ( 'NONE', ( #14825, #2145, #17635, #3913 ) ) ;
#9820 = ADVANCED_FACE ( 'NONE', ( #5615 ), #8303, .F. ) ;
#9821 = LINE ( 'NONE', #12788, #18031 ) ;
#9822 = VECTOR ( 'NONE', #3448, 1000.000000000000114 ) ;
#9823 = CARTESIAN_POINT ( 'NONE',  ( 1.027846397803542144, 18.74680007765648071, -3.346150245485522312 ) ) ;
#9824 = EDGE_CURVE ( 'NONE', #15656, #8139, #11259, .T. ) ;
#9825 =( GEOMETRIC_REPRESENTATION_CONTEXT ( 3 ) GLOBAL_UNCERTAINTY_ASSIGNED_CONTEXT ( ( #9528 ) ) GLOBAL_UNIT_ASSIGNED_CONTEXT ( ( #1465, #13973, #12574 ) ) REPRESENTATION_CONTEXT ( 'NONE', 'WORKASPACE' ) );
#9826 = CARTESIAN_POINT ( 'NONE',  ( 4.243569643750003451, -20.93616690305174544, -9.889955075634029313 ) ) ;
#9827 = EDGE_CURVE ( 'NONE', #1204, #8695, #8460, .T. ) ;
#9828 = CARTESIAN_POINT ( 'NONE',  ( -1.734723475976807094E-15, 27.59999999999999432, -10.50000000000000178 ) ) ;
#9829 = EDGE_CURVE ( 'NONE', #14557, #5353, #5707, .T. ) ;
#9830 = DIRECTION ( 'NONE',  ( -0.000000000000000000, -0.5735764363510414965, -0.8191520442889950182 ) ) ;
#9831 = DIRECTION ( 'NONE',  ( -0.000000000000000000, 1.000000000000000000, -0.000000000000000000 ) ) ;
#9832 = EDGE_LOOP ( 'NONE', ( #17262, #14145, #13954, #4339 ) ) ;
#9833 = ORIENTED_EDGE ( 'NONE', *, *, #2991, .T. ) ;
#9834 = CARTESIAN_POINT ( 'NONE',  ( -2.115076519116362519, 20.12180007765648071, 3.012182706137107147 ) ) ;
#9835 = DIRECTION ( 'NONE',  ( 0.000000000000000000, 0.000000000000000000, -1.000000000000000000 ) ) ;
#9836 = CARTESIAN_POINT ( 'NONE',  ( -1.734723475976807094E-15, 31.99999999999999289, -2.500000000000000000 ) ) ;
#9837 = DIRECTION ( 'NONE',  ( 0.000000000000000000, -1.000000000000000000, 0.000000000000000000 ) ) ;
#9838 = CARTESIAN_POINT ( 'NONE',  ( -1.999999999999996225, -24.09004865885014723, -16.16215176765433270 ) ) ;
#9839 = VERTEX_POINT ( 'NONE', #6162 ) ;
#9840 = CIRCLE ( 'NONE', #18172, 2.149999999999995470 ) ;
#9841 = CARTESIAN_POINT ( 'NONE',  ( -2.864755990943222308, 16.75319992234354416, 2.011557305968548093 ) ) ;
#9842 = CARTESIAN_POINT ( 'NONE',  ( -5.330712181944245322E-15, -26.52681618229254212, -5.059759365251903951 ) ) ;
#9843 = CARTESIAN_POINT ( 'NONE',  ( -0.05938372350927861171, 33.62180007765648071, -3.680117784833935701 ) ) ;
#9844 =( REPRESENTATION_RELATIONSHIP ('NONE','NONE', #15868, #1416 ) REPRESENTATION_RELATIONSHIP_WITH_TRANSFORMATION ( #5512 )SHAPE_REPRESENTATION_RELATIONSHIP( ) );
#9845 = CARTESIAN_POINT ( 'NONE',  ( -2.211161402132839182, 24.12819992234354416, 2.942372952327218627 ) ) ;
#9846 = FACE_OUTER_BOUND ( 'NONE', #4142, .T. ) ;
#9847 = CARTESIAN_POINT ( 'NONE',  ( 9.999999999999998224, 16.59999999999999787, -2.500000000000001776 ) ) ;
#9848 = CARTESIAN_POINT ( 'NONE',  ( -5.330712181944245322E-15, -28.62395502770104017, -8.054784027183542250 ) ) ;
#9849 = AXIS2_PLACEMENT_3D ( 'NONE', #12460, #15174, #17793 ) ;
#9850 = COLOUR_RGB ( '',0.8941176470588234615, 0.8941176470588234615, 0.8941176470588234615 ) ;
#9851 = CARTESIAN_POINT ( 'NONE',  ( 0.9964672492349638810, -9.999999999997456257, -3.740800554891051899 ) ) ;
#9852 = CARTESIAN_POINT ( 'NONE',  ( -3.706921591972381904E-14, -17.47795000513098884, -7.653406576829588026 ) ) ;
#9853 = DIRECTION ( 'NONE',  ( 0.000000000000000000, -1.000000000000000000, 0.000000000000000000 ) ) ;
#9854 = CARTESIAN_POINT ( 'NONE',  ( -4.243569643750005227, -21.98179658260448832, -2.840288794994898058 ) ) ;
#9855 = CARTESIAN_POINT ( 'NONE',  ( -10.00000000000000178, 18.79999999999999361, -2.500000000000001776 ) ) ;
#9856 = VERTEX_POINT ( 'NONE', #10043 ) ;
#9857 = CARTESIAN_POINT ( 'NONE',  ( 0.05938372350921204690, 17.62819992234354416, -2.628655560595669183 ) ) ;
#9858 = CARTESIAN_POINT ( 'NONE',  ( 4.243569643749996345, -28.34849502610105176, -11.93287648660273703 ) ) ;
#9859 = PLANE ( 'NONE',  #6573 ) ;
#9860 = AXIS2_PLACEMENT_3D ( 'NONE', #8223, #5446, #13887 ) ;
#9861 = CARTESIAN_POINT ( 'NONE',  ( -9.670852723135475060, -9.962926482346835755, 0.1910560633138593534 ) ) ;
#9862 = ADVANCED_FACE ( 'NONE', ( #4402 ), #15817, .F. ) ;
#9863 = ORIENTED_EDGE ( 'NONE', *, *, #7498, .T. ) ;
#9864 = CARTESIAN_POINT ( 'NONE',  ( 3.250767888004682415, -21.90484815091188509, -2.246271217071878379 ) ) ;
#9865 = CARTESIAN_POINT ( 'NONE',  ( -2.864755990943265829, 35.74680007765648071, -2.011557305968488141 ) ) ;
#9866 = CARTESIAN_POINT ( 'NONE',  ( -1.734723475976807094E-15, 29.79999999999999716, -11.50000000000000178 ) ) ;
#9867 = CARTESIAN_POINT ( 'NONE',  ( 4.243569643750000786, -25.80382324818726048, -12.57019867080359710 ) ) ;
#9868 = DIRECTION ( 'NONE',  ( 0.000000000000000000, 0.000000000000000000, -1.000000000000000000 ) ) ;
#9869 = VECTOR ( 'NONE', #7252, 1000.000000000000000 ) ;
#9870 = CARTESIAN_POINT ( 'NONE',  ( 4.299564228933482956E-15, -19.22018842984233089, -10.14158091035064579 ) ) ;
#9871 = DIRECTION ( 'NONE',  ( 0.000000000000000000, 0.000000000000000000, -1.000000000000000000 ) ) ;
#9872 = CARTESIAN_POINT ( 'NONE',  ( 2.121784821874994176, -27.56671030237578179, -8.680627135892345692 ) ) ;
#9873 = VERTEX_POINT ( 'NONE', #15720 ) ;
#9874 = FACE_OUTER_BOUND ( 'NONE', #6207, .T. ) ;
#9875 = CARTESIAN_POINT ( 'NONE',  ( -1.999999999999996225, -17.63731374990092959, -6.946691269403138413 ) ) ;
#9876 = CARTESIAN_POINT ( 'NONE',  ( -0.8262555684461330152, 15.99680007765648249, -2.360188852285403982 ) ) ;
#9877 = ORIENTED_EDGE ( 'NONE', *, *, #17903, .T. ) ;
#9878 = CARTESIAN_POINT ( 'NONE',  ( 4.299564228933482956E-15, -19.02660638327880349, -9.865117096409875330 ) ) ;
#9879 = ADVANCED_FACE ( 'NONE', ( #10230 ), #8183, .T. ) ;
#9880 = EDGE_CURVE ( 'NONE', #17896, #8888, #333, .T. ) ;
#9881 = SHAPE_REPRESENTATION_RELATIONSHIP ( 'NONE' , 'NONE' ,  #1416, #10928 ) ;
#9882 = DIRECTION ( 'NONE',  ( -0.000000000000000000, 1.000000000000000000, -0.000000000000000000 ) ) ;
#9883 = EDGE_CURVE ( 'NONE', #9839, #11183, #17978, .T. ) ;
#9884 = CARTESIAN_POINT ( 'NONE',  ( -1.497042530366522461, 32.37819992234353350, -2.161531897785030409 ) ) ;
#9885 = ORIENTED_EDGE ( 'NONE', *, *, #1672, .T. ) ;
#9886 = CARTESIAN_POINT ( 'NONE',  ( -2.121784821874996396, -21.19097827587949467, -12.38960848565391260 ) ) ;
#9887 = CARTESIAN_POINT ( 'NONE',  ( -3.607379964056306676, 32.74680007765648071, 2.690724712371306282 ) ) ;
#9888 = ORIENTED_EDGE ( 'NONE', *, *, #592, .T. ) ;
#9889 = CYLINDRICAL_SURFACE ( 'NONE', #14603, 4.000000000000000000 ) ;
#9890 = SURFACE_STYLE_USAGE ( .BOTH. , #2781 ) ;
#9891 = CARTESIAN_POINT ( 'NONE',  ( 4.000000000000000888, -22.04510516337187198, -7.202192930068894938 ) ) ;
#9892 = FACE_OUTER_BOUND ( 'NONE', #8999, .T. ) ;
#9893 =( BOUNDED_CURVE ( )  B_SPLINE_CURVE ( 2, ( #3229, #72, #5727, #14542, #11736, #11367, #17146, #12945, #8767 ),
 .UNSPECIFIED., .F., .T. ) 
 B_SPLINE_CURVE_WITH_KNOTS ( ( 3, 2, 2, 2, 3 ),
 ( 0.9224137931034482873, 0.9252873563218391162, 0.9310344827586206629, 0.9367816091954023205, 0.9396551724137931494 ),
 .UNSPECIFIED. ) 
 CURVE ( )  GEOMETRIC_REPRESENTATION_ITEM ( )  RATIONAL_B_SPLINE_CURVE ( ( 0.9330127018922194093, 0.9330127018922194093, 1.000000000000000000, 0.8660254037844387076, 1.000000000000000000, 0.8660254037844387076, 1.000000000000000000, 0.9330127018922180770, 0.9330127018922194093 ) ) 
 REPRESENTATION_ITEM ( '' )  );
#9894 = CARTESIAN_POINT ( 'NONE',  ( 4.730628863548789710E-15, -18.66035907967750163, -10.91125478059535681 ) ) ;
#9895 = ORIENTED_EDGE ( 'NONE', *, *, #7963, .T. ) ;
#9896 = DIRECTION ( 'NONE',  ( -0.000000000000000000, -1.000000000000000000, -0.000000000000000000 ) ) ;
#9897 = ORIENTED_EDGE ( 'NONE', *, *, #12881, .F. ) ;
#9898 = CARTESIAN_POINT ( 'NONE',  ( 1.999999999999994449, -26.79704244006331493, -7.949185819321580304 ) ) ;
#9899 = DIRECTION ( 'NONE',  ( -0.000000000000000000, -0.5735764363510414965, -0.8191520442889950182 ) ) ;
#9900 = DIRECTION ( 'NONE',  ( -0.000000000000000000, 1.000000000000000000, -0.000000000000000000 ) ) ;
#9901 = SHAPE_REPRESENTATION_RELATIONSHIP ( 'NONE' , 'NONE' ,  #12769, #5178 ) ;
#9902 = CARTESIAN_POINT ( 'NONE',  ( -1.336863392178569088, 20.00319992234354416, -4.297206761780648421 ) ) ;
#9903 = CARTESIAN_POINT ( 'NONE',  ( -3.518350579753606322, 24.37819992234354061, 1.080741659609877781 ) ) ;
#9904 = CARTESIAN_POINT ( 'NONE',  ( 1.999999999999994449, -28.86191761092706187, -10.89813317876196308 ) ) ;
#9905 = CARTESIAN_POINT ( 'NONE',  ( -0.7188294034286550893, 15.00319992234354594, -2.395093729190349130 ) ) ;
#9906 = CARTESIAN_POINT ( 'NONE',  ( -3.607379964056363075, 29.75319992234354416, -2.690724712371229899 ) ) ;
#9907 = CARTESIAN_POINT ( 'NONE',  ( 2.000000000000004441, -21.22933618184438842, -12.07663094575620377 ) ) ;
#9908 = ORIENTED_EDGE ( 'NONE', *, *, #15116, .T. ) ;
#9909 = EDGE_CURVE ( 'NONE', #17255, #4281, #14522, .T. ) ;
#9910 = CARTESIAN_POINT ( 'NONE',  ( 12.00000000000000178, 13.00000000000000178, -15.00000000000000000 ) ) ;
#9911 = CARTESIAN_POINT ( 'NONE',  ( 1.135272562821090458, 22.24680007765648071, 3.311245368580554072 ) ) ;
#9912 = CARTESIAN_POINT ( 'NONE',  ( 9.670609637961767646, -9.962952946793892650, 0.1891778739417505906 ) ) ;
#9913 = CARTESIAN_POINT ( 'NONE',  ( 4.730628863548789710E-15, -18.62809540513275053, -10.86517747810410128 ) ) ;
#9914 = CARTESIAN_POINT ( 'NONE',  ( 4.481649420246366589, 24.12180007765647716, -1.518615910253458212 ) ) ;
#9915 = CARTESIAN_POINT ( 'NONE',  ( -2.000000000000005773, -26.32384188007369730, -7.273385382783162711 ) ) ;
#9916 = LINE ( 'NONE', #15423, #13565 ) ;
#9917 = ORIENTED_EDGE ( 'NONE', *, *, #10393, .F. ) ;
#9918 = ORIENTED_EDGE ( 'NONE', *, *, #13173, .T. ) ;
#9919 = CARTESIAN_POINT ( 'NONE',  ( -0.05938372350927861171, 21.12180007765648071, -3.680117784833935701 ) ) ;
#9920 = DIRECTION ( 'NONE',  ( -0.000000000000000000, -1.000000000000000000, -0.000000000000000000 ) ) ;
#9921 = SURFACE_STYLE_FILL_AREA ( #2983 ) ;
#9922 = PLANE ( 'NONE',  #8052 ) ;
#9923 = CARTESIAN_POINT ( 'NONE',  ( 4.000000000000000888, -22.88396070224021273, -8.400202795848317194 ) ) ;
#9924 = VERTEX_POINT ( 'NONE', #16006 ) ;
#9925 = CARTESIAN_POINT ( 'NONE',  ( -1.027846397803611866, 22.50319992234354416, -3.346150245485499219 ) ) ;
#9926 = CARTESIAN_POINT ( 'NONE',  ( 4.243569643750000786, -22.96461988824960443, -8.515396051573073777 ) ) ;
#9927 =( BOUNDED_CURVE ( )  B_SPLINE_CURVE ( 1, ( #988, #12188 ),
 .UNSPECIFIED., .F., .T. ) 
 B_SPLINE_CURVE_WITH_KNOTS ( ( 2, 2 ),
 ( 0.000000000000000000, 1.000000000000000000 ),
 .UNSPECIFIED. ) 
 CURVE ( )  GEOMETRIC_REPRESENTATION_ITEM ( )  RATIONAL_B_SPLINE_CURVE ( ( 0.9401540970596700131, 0.9401540970596700131 ) ) 
 REPRESENTATION_ITEM ( '' )  );
#9928 = CARTESIAN_POINT ( 'NONE',  ( 2.500000000000001332, 16.74680007765648071, -0.05647727720535888202 ) ) ;
#9929 = EDGE_CURVE ( 'NONE', #7280, #5293, #13020, .T. ) ;
#9930 = CARTESIAN_POINT ( 'NONE',  ( -1.135272562821019626, 31.50319992234354416, 3.311245368580577164 ) ) ;
#9931 = CARTESIAN_POINT ( 'NONE',  ( 12.00000000000000178, 48.00000000000000000, 15.00000000000000000 ) ) ;
#9932 = CARTESIAN_POINT ( 'NONE',  ( -9.000000000000001776, 23.19999999999999574, 2.499999999999995559 ) ) ;
#9933 = CONICAL_SURFACE ( 'NONE', #10229, 1732.050807568857181, 1.047197551196592746 ) ;
#9934 = ADVANCED_FACE ( 'NONE', ( #6254 ), #7637, .F. ) ;
#9935 = CARTESIAN_POINT ( 'NONE',  ( -2.121784821875005722, -25.57711703878310061, -5.839193482264897206 ) ) ;
#9936 = CIRCLE ( 'NONE', #12308, 4.000000000000000000 ) ;
#9937 = CARTESIAN_POINT ( 'NONE',  ( -13.00000000000000178, 13.00000000000000178, 25.00000000000000355 ) ) ;
#9938 = FACE_OUTER_BOUND ( 'NONE', #16729, .T. ) ;
#9939 = CARTESIAN_POINT ( 'NONE',  ( -4.000000000000004441, -22.81838172630220640, -4.280228404999725456 ) ) ;
#9940 = CARTESIAN_POINT ( 'NONE',  ( 4.243569643749996345, -22.41197890986777352, -3.454652828211636884 ) ) ;
#9941 = FACE_OUTER_BOUND ( 'NONE', #3098, .T. ) ;
#9942 = ORIENTED_EDGE ( 'NONE', *, *, #8857, .F. ) ;
#9943 = CARTESIAN_POINT ( 'NONE',  ( 0.7188294034286553114, 23.75319992234354771, 2.395093729190349130 ) ) ;
#9944 = AXIS2_PLACEMENT_3D ( 'NONE', #9416, #10994, #15094 ) ;
#9945 = CARTESIAN_POINT ( 'NONE',  ( 4.243569643750003451, -24.80780784842128028, -15.41923137458474535 ) ) ;
#9946 = CARTESIAN_POINT ( 'NONE',  ( 8.000000000000001776, 31.99999999999999289, -2.500000000000002220 ) ) ;
#9947 = ADVANCED_FACE ( 'NONE', ( #614 ), #7283, .T. ) ;
#9948 = DIRECTION ( 'NONE',  ( 1.000000000000000000, 0.000000000000000000, 0.000000000000000000 ) ) ;
#9949 = ORIENTED_EDGE ( 'NONE', *, *, #3443, .T. ) ;
#9950 = CARTESIAN_POINT ( 'NONE',  ( 4.243569643750003451, -18.38733661401680308, -6.249848178824808365 ) ) ;
#9951 = CARTESIAN_POINT ( 'NONE',  ( -1.027846397803541700, 32.49680007765648071, 3.346150245485522312 ) ) ;
#9952 =( NAMED_UNIT ( * ) SI_UNIT ( $, .STERADIAN. ) SOLID_ANGLE_UNIT ( ) );
#9953 = VECTOR ( 'NONE', #8284, 1000.000000000000000 ) ;
#9954 = CARTESIAN_POINT ( 'NONE',  ( -2.121784821874996396, -22.44926158312459208, -14.18662328281289398 ) ) ;
#9955 = DIRECTION ( 'NONE',  ( -4.915049848600951133E-16, 0.000000000000000000, -1.000000000000000000 ) ) ;
#9956 = CARTESIAN_POINT ( 'NONE',  ( 8.399999999999998579, 0.000000000000000000, 4.000000000000001776 ) ) ;
#9957 = DIRECTION ( 'NONE',  ( -1.000000000000000000, -0.000000000000000000, -0.000000000000000000 ) ) ;
#9958 = CARTESIAN_POINT ( 'NONE',  ( -4.243569643750005227, -26.36965632068995191, -9.106801933805707350 ) ) ;
#9959 = B_SPLINE_CURVE_WITH_KNOTS ( 'NONE', 3,
 ( #14952, #2245, #934, #665, #6489, #13529, #4914, #10566, #6577, #12135, #17828, #5093, #10751, #16426, #13990, #9628, #12412, #2517 ),
 .UNSPECIFIED., .F., .F.,
 ( 4, 2, 2, 2, 2, 2, 2, 2, 4 ),
 ( 0.000000000000000000, 0.0009265903667615439090, 0.001853180733523087818, 0.002779771100284632052, 0.003706361467046175636, 0.004632951833807719653, 0.005559542200569264105, 0.006486132567330806821, 0.007412722934092349537 ),
 .UNSPECIFIED. ) ;
#9960 = DIRECTION ( 'NONE',  ( -3.373073425510457965E-16, 0.000000000000000000, -1.000000000000000000 ) ) ;
#9961 = CARTESIAN_POINT ( 'NONE',  ( -1.999999999999996225, -17.12109495718499375, -6.209454429543042941 ) ) ;
#9962 = CARTESIAN_POINT ( 'NONE',  ( -0.8262555684461330152, 20.99680007765648071, -2.360188852285403982 ) ) ;
#9963 = VERTEX_POINT ( 'NONE', #11624 ) ;
#9964 = CYLINDRICAL_SURFACE ( 'NONE', #14293, 4.000000000000000000 ) ;
#9965 = PLANE ( 'NONE',  #6331 ) ;
#9966 = AXIS2_PLACEMENT_3D ( 'NONE', #14453, #10538, #3418 ) ;
#9967 = CARTESIAN_POINT ( 'NONE',  ( 2.481649420246391902, 38.37819992234354061, 0.8687765177875720335 ) ) ;
#9968 = ORIENTED_EDGE ( 'NONE', *, *, #1923, .T. ) ;
#9969 = CARTESIAN_POINT ( 'NONE',  ( 4.243569643750003451, -21.74275876667040208, -11.04188763791542982 ) ) ;
#9970 = CARTESIAN_POINT ( 'NONE',  ( 1.336863392178479160, 31.24680007765648071, -4.297206761780677731 ) ) ;
#9971 = ORIENTED_EDGE ( 'NONE', *, *, #3663, .T. ) ;
#9972 = PRESENTATION_STYLE_ASSIGNMENT (( #17242 ) ) ;
#9973 = CARTESIAN_POINT ( 'NONE',  ( 1.071796769724485232, -26.14904217797241515, -6.089435214781468986 ) ) ;
#9974 = ADVANCED_FACE ( 'NONE', ( #6063 ), #11716, .F. ) ;
#9975 = VECTOR ( 'NONE', #4611, 1000.000000000000000 ) ;
#9976 = CARTESIAN_POINT ( 'NONE',  ( 0.000000000000000000, 31.99999999999999289, 2.500000000000000000 ) ) ;
#9977 = EDGE_CURVE ( 'NONE', #17729, #16267, #3746, .T. ) ;
#9979 = DIRECTION ( 'NONE',  ( -1.000000000000000000, -0.000000000000000000, -0.000000000000000000 ) ) ;
#9978 = CIRCLE ( 'NONE', #14758, 0.9999999999999991118 ) ;
#9980 = CARTESIAN_POINT ( 'NONE',  ( -2.121784821875005722, -24.02846066063528596, -3.627482962684610346 ) ) ;
#9981 = ORIENTED_EDGE ( 'NONE', *, *, #13298, .T. ) ;
#9982 = ADVANCED_FACE ( 'NONE', ( #7264 ), #5881, .F. ) ;
#9983 = CARTESIAN_POINT ( 'NONE',  ( -9.000000000000001776, 34.19999999999999574, 2.499999999999995559 ) ) ;
#9984 = VERTEX_POINT ( 'NONE', #14421 ) ;
#9985 = EDGE_LOOP ( 'NONE', ( #8230, #17134, #6097, #11274, #5487, #11548, #7353, #3770 ) ) ;
#9986 = CARTESIAN_POINT ( 'NONE',  ( 1.820000000000000062, 0.000000000000000000, 0.000000000000000000 ) ) ;
#9987 = CARTESIAN_POINT ( 'NONE',  ( -1.071796769724496334, -29.01129893934772852, -10.17716150332382696 ) ) ;
#9988 = ADVANCED_FACE ( 'NONE', ( #4494 ), #16189, .T. ) ;
#9989 = CARTESIAN_POINT ( 'NONE',  ( -4.481649420246396787, 14.62819992234354594, -1.518615910253363399 ) ) ;
#9990 = CARTESIAN_POINT ( 'NONE',  ( 2.798362969681409851, 31.00319992234354416, 2.102939460078764977 ) ) ;
#9991 = CARTESIAN_POINT ( 'NONE',  ( -1.497042530366477164, 37.62180007765646650, 2.161531897785062384 ) ) ;
#9992 = ORIENTED_EDGE ( 'NONE', *, *, #15884, .F. ) ;
#9993 = AXIS2_PLACEMENT_3D ( 'NONE', #10310, #11514, #11610 ) ;
#9994 = CARTESIAN_POINT ( 'NONE',  ( 3.673772985318163098, 30.50319992234354416, -2.599342558261029001 ) ) ;
#9995 = AXIS2_PLACEMENT_3D ( 'NONE', #10405, #13281, #213 ) ;
#9996 = CARTESIAN_POINT ( 'NONE',  ( 4.000000000000000888, -24.10998033423561893, -10.15114028950927683 ) ) ;
#9997 = VERTEX_POINT ( 'NONE', #234 ) ;
#9998 = EDGE_CURVE ( 'NONE', #6301, #14557, #1855, .T. ) ;
#9999 = CARTESIAN_POINT ( 'NONE',  ( -3.706921591972381904E-14, -17.47795000513098884, -7.653406576829588026 ) ) ;
#10000 = CARTESIAN_POINT ( 'NONE',  ( -2.864755990943265829, 30.74680007765647716, -2.011557305968488141 ) ) ;
#10001 =( BOUNDED_SURFACE ( )  B_SPLINE_SURFACE ( 1, 2, ( 
 ( #8538, #12896, #11597, #3085, #14391, #1697, #305, #5947, #17294, #7427, #4561, #3178, #13085, #16343, #10491, #17381, #16164, #8912, #3275, #14589, #10581, #9012, #10396, #11690, #7800, #14779, #4842, #4647, #4928, #6414, #2076, #10299, #15979, #1893, #588, #7524, #13178, #9283, #3457, #9100, #2170, #6230, #7706, #489, #6132, #11783, #13457, #17666, #2258, #11974, #17478, #16257, #11878, #13271, #16074, #4747, #3548, #17573, #3636, #769, #10673, #14963, #13366, #9193, #3368, #14874, #14688, #5018, #680, #12059, #17756, #6326, #7883, #13542, #6040, #1985, #7611, #13729, #16718, #10945, #12150, #12240, #18209, #13635, #9368, #17841, #6503, #18020, #15414, #1225, #4079, #15045, #6594, #2618, #17929, #13822, #16630, #1039, #9732, #11036, #6679, #8158, #16529, #5106, #3993, #5474, #5292, #2710, #8341, #13915, #857, #16440, #3903, #10765, #6767, #3718, #8258, #11120, #2350, #5201, #12332, #9552, #15230, #9640, #7981, #16808, #948, #10852, #2529, #3807, #9462, #15135, #1132, #2438, #8068, #12424, #18117, #5385, #15318, #6860, #12517, #5563, #6948, #14090, #9996, #2969, #9907, #15579, #10180, #12785, #15857, #14185, #1401, #2796, #14369, #4265, #8427, #5745, #2879, #8511, #1489, #11569, #1315, #3062, #4176, #5923, #93, #12600, #11385, #16899, #11210, #9818, #12966, #8601, #8694, #11477, #7033, #1670, #7217, #15501, #18291, #12695, #2, #5653, #11295, #16989, #14003, #7124, #7304, #17074, #4538, #4347, #15761, #15670, #14277, #1582, #12872, #179, #5829, #280, #17168, #3154, #4442, #10083, #17264, #14662, #13154, #566, #6206, #11854, #10554, #6015, #4819, #465, #6300, #10371, #10468, #14472, #17454, #6393, #16145, #8989, #16229, #6108, #16323, #3524, #13062, #14851, #9171, #17728, #11667, #373, #13345, #1866, #17551, #4721, #1772, #748, #3434, #1961, #17360, #17646, #13246, #12036, #4904, #14566, #16051, #9075, #8887, #7587, #7683, #7496, #14754, #4996, #15955, #2144, #10651, #3342, #11759, #2054, #656, #11953, #7774, #13435, #8788, #7402, #4625, #10272, #3249, #17907, #5451, #3610, #9258, #6839, #13799, #15024, #1107, #13611, #2596, #2414, #8138, #6747, #3880, #11098, #9529, #14944, #6660, #2236, #16506, #12403, #13706, #7862, #2324, #8229, #16416, #12127, #13520, #834, #8045, #18182, #3970, #12490, #17821, #9346, #5365, #7955, #16606, #1020, #3785, #6476, #18094, #9438, #10925, #925, #5083, #11012, #13892, #12309, #10742, #3699, #16691, #6568, #12219, #17999, #5175, #15208, #10831, #9621, #1203, #15111, #5270, #2510, #15297, #10133, #8840, #7544, #3295, #9705, #4054, #15813, #7173, #15389, #135, #11526, #11429, #8934, #14234, #14615, #230 ),
 ( #3200, #1624, #3016, #2689, #423, #7356, #3110, #8320, #15903, #17406, #13016, #1537, #12832, #5787, #17218, #17120, #4399, #1916, #8740, #1721, #13110, #4490, #329, #10039, #15716, #8650, #6060, #10225, #13199, #4580, #14327, #14517, #14415, #5879, #7258, #12918, #1816, #5965, #514, #11712, #6158, #16785, #11621, #7451, #17314, #4669, #10322, #16002, #977, #17686, #16180, #3569, #9218, #14896, #13564, #9029, #7820, #3477, #9304, #13387, #13476, #17503, #2098, #9389, #788, #11992, #881, #9122, #11806, #6524, #16099, #17865, #12176, #2374, #14708, #3390, #16371, #4863, #2194, #7726, #4767, #3741, #6435, #4948, #2005, #2279, #16280, #15069, #7908, #17599, #702, #12081, #11900, #10604, #10697, #10512, #17781, #8002, #607, #5131, #13658, #6350, #14801, #5041, #3657, #14980, #10785, #16459, #10418, #7633, #13297, #6251, #5412, #2554, #8448, #6622, #12266, #9848, #16837, #18048, #2821, #11062, #14119, #6798, #12354, #13756, #6971, #15258, #1066, #16744, #8185, #1155, #13844, #4201, #17951, #14031, #15159, #16925, #4019, #5224, #9666, #9483, #3836, #2466, #5593, #1251, #1339, #4107, #6700, #12630, #18231, #8094, #10876, #16557, #5321, #10974, #16653, #3927, #9579, #12449, #18319, #18145, #15524, #15342, #8368, #2642, #8283, #13941, #6884, #12542, #5499, #11237, #11146, #9758, #15439, #2735, #14304, #7149, #10022, #4371, #12994, #15697, #15882, #11503, #10111, #1605, #1796, #206, #2996, #3277, #17382, #11599, #8627, #17295, #11409, #402, #5857, #5948, #4563, #1698, #8913, #7332, #1431, #4469, #7059, #7240, #10202, #17197, #12727, #12812, #6041, #14213, #9935, #27, #5680, #15792, #15981, #7428, #4648, #15604, #118, #3179, #5770, #14393, #3086, #12898, #10300, #8817, #8720, #306, #17102, #11323, #14498, #11692, #13087, #17018, #4288, #2905, #8540, #1517, #682, #1894, #2171, #7526, #3639, #859, #492, #13273, #2078, #4930, #7708, #6415, #5109, #6506, #13179, #6133, #13367, #4748, #11784, #16076, #9102, #9013, #12153, #17480, #17843, #16165, #13544, #6328, #10398, #3369, #14689, #1987, #10583, #3550, #10492, #3458, #770, #17576, #590, #7612, #16345, #16259, #11975, #6232, #13459, #14965, #9194, #11879, #4843, #14780, #17667, #14875, #7801, #10767, #12060, #17758, #10675, #5022, #9285, #2261, #7885, #16442, #3721, #14591, #15137, #11212, #6770, #5204, #16902, #15233, #13731, #1134, #12428, #18120, #11123, #6596, #5388, #1042, #6863, #10948, #11039, #15047, #18022, #6950, #16721, #9555, #16811, #6681, #9371, #4081, #13637, #15417, #9734, #18294, #12242, #951, #13918, #2440, #3996, #5295, #2353, #1317, #9642, #2531, #17931, #18211, #13824, #12604, #5478 ) ),
 .UNSPECIFIED., .F., .F., .T. ) 
 B_SPLINE_SURFACE_WITH_KNOTS ( ( 2, 2 ),
 ( 3, 2, 2, 2, 2, 2, 2, 2, 2, 2, 2, 2, 2, 2, 2, 2, 2, 2, 2, 2, 2, 2, 2, 2, 2, 2, 2, 2, 2, 2, 2, 2, 2, 2, 2, 2, 2, 2, 2, 2, 2, 2, 2, 2, 2, 2, 2, 2, 2, 2, 2, 2, 2, 2, 2, 2, 2, 2, 2, 2, 2, 2, 2, 2, 2, 2, 2, 2, 2, 2, 2, 2, 2, 2, 2, 2, 2, 2, 2, 2, 2, 2, 2, 2, 2, 2, 2, 2, 2, 2, 2, 2, 2, 2, 2, 2, 2, 2, 2, 2, 2, 2, 2, 2, 2, 2, 2, 2, 2, 2, 2, 2, 2, 2, 2, 2, 2, 2, 2, 2, 2, 2, 2, 2, 2, 2, 2, 2, 2, 2, 2, 2, 2, 2, 2, 2, 2, 2, 2, 2, 2, 2, 2, 2, 2, 2, 2, 2, 2, 2, 2, 2, 2, 2, 2, 2, 2, 2, 2, 2, 2, 2, 2, 2, 2, 2, 2, 2, 2, 2, 2, 2, 2, 2, 3 ),
 ( 0.000000000000000000, 1.000000000000000000 ),
 ( 0.000000000000000000, 0.005747126436781609116, 0.01149425287356321823, 0.01724137931034482735, 0.02298850574712643646, 0.02873563218390804558, 0.03448275862068965469, 0.04022988505747126381, 0.04597701149425287293, 0.05172413793103448204, 0.05747126436781609116, 0.06321839080459770721, 0.06896551724137930939, 0.07471264367816092544, 0.08045977011494252762, 0.08620689655172414367, 0.09195402298850574585, 0.09770114942528736190, 0.1034482758620689641, 0.1091954022988505801, 0.1149425287356321823, 0.1206896551724137984, 0.1264367816091954144, 0.1321839080459770166, 0.1379310344827586188, 0.1436781609195402210, 0.1494252873563218509, 0.1551724137931034531, 0.1609195402298850552, 0.1666666666666666574, 0.1724137931034482873, 0.1781609195402298895, 0.1839080459770114917, 0.1896551724137930939, 0.1954022988505747238, 0.2011494252873563260, 0.2068965517241379282, 0.2126436781609195303, 0.2183908045977011603, 0.2241379310344827624, 0.2298850574712643646, 0.2356321839080459668, 0.2413793103448275967, 0.2471264367816091989, 0.2528735632183908288, 0.2586206896551724310, 0.2643678160919540332, 0.2701149425287356354, 0.2758620689655172376, 0.2816091954022988397, 0.2873563218390804419, 0.2931034482758620441, 0.2988505747126437018, 0.3045977011494253039, 0.3103448275862069061, 0.3160919540229885083, 0.3218390804597701105, 0.3275862068965517127, 0.3333333333333333148, 0.3390804597701149170, 0.3448275862068965747, 0.3505747126436781769, 0.3563218390804597790, 0.3620689655172413812, 0.3678160919540229834, 0.3735632183908045856, 0.3793103448275861878, 0.3850574712643677899, 0.3908045977011494476, 0.3965517241379310498, 0.4022988505747126520, 0.4080459770114942541, 0.4137931034482758563, 0.4195402298850574585, 0.4252873563218390607, 0.4310344827586206629, 0.4367816091954023205, 0.4425287356321839227, 0.4482758620689655249, 0.4540229885057471271, 0.4597701149425287293, 0.4655172413793103314, 0.4712643678160919336, 0.4770114942528735358, 0.4827586206896551935, 0.4885057471264367956, 0.4942528735632183978, 0.5000000000000000000, 0.5057471264367816577, 0.5114942528735632044, 0.5172413793103448620, 0.5229885057471264087, 0.5287356321839080664, 0.5344827586206896131, 0.5402298850574712707, 0.5459770114942529284, 0.5517241379310344751, 0.5574712643678161328, 0.5632183908045976795, 0.5689655172413793371, 0.5747126436781608838, 0.5804597701149425415, 0.5862068965517240882, 0.5919540229885057459, 0.5977011494252874035, 0.6034482758620689502, 0.6091954022988506079, 0.6149425287356321546, 0.6206896551724138122, 0.6264367816091953589, 0.6321839080459770166, 0.6379310344827586743, 0.6436781609195402210, 0.6494252873563218786, 0.6551724137931034253, 0.6609195402298850830, 0.6666666666666666297, 0.6724137931034482873, 0.6781609195402298340, 0.6839080459770114917, 0.6896551724137931494, 0.6954022988505746961, 0.7011494252873563537, 0.7068965517241379004, 0.7126436781609195581, 0.7183908045977011048, 0.7241379310344827624, 0.7298850574712644201, 0.7356321839080459668, 0.7413793103448276245, 0.7471264367816091712, 0.7528735632183908288, 0.7586206896551723755, 0.7643678160919540332, 0.7701149425287355799, 0.7758620689655172376, 0.7816091954022988952, 0.7873563218390804419, 0.7931034482758620996, 0.7988505747126436463, 0.8045977011494253039, 0.8103448275862068506, 0.8160919540229885083, 0.8218390804597701660, 0.8275862068965517127, 0.8333333333333333703, 0.8390804597701149170, 0.8448275862068965747, 0.8505747126436781214, 0.8563218390804597790, 0.8620689655172413257, 0.8678160919540229834, 0.8735632183908046411, 0.8793103448275861878, 0.8850574712643678454, 0.8908045977011493921, 0.8965517241379310498, 0.9022988505747125965, 0.9080459770114942541, 0.9137931034482759118, 0.9195402298850574585, 0.9252873563218391162, 0.9310344827586206629, 0.9367816091954023205, 0.9425287356321838672, 0.9482758620689655249, 0.9540229885057470716, 0.9597701149425287293, 0.9655172413793103869, 0.9712643678160919336, 0.9770114942528735913, 0.9827586206896551380, 0.9885057471264367956, 0.9942528735632183423, 0.9961881933054925753 ),
 .UNSPECIFIED. ) 
 GEOMETRIC_REPRESENTATION_ITEM ( )  RATIONAL_B_SPLINE_SURFACE ( (
 ( 1.000000000000000000, 0.8660254037844387076, 1.000000000000000000, 0.8660254037844387076, 1.000000000000000000, 0.8660254037844387076, 1.000000000000000000, 0.8660254037844387076, 1.000000000000000000, 0.8660254037844387076, 1.000000000000000000, 0.8660254037844387076, 1.000000000000000000, 0.8660254037844387076, 1.000000000000000000, 0.8660254037844387076, 1.000000000000000000, 0.8660254037844387076, 1.000000000000000000, 0.8660254037844387076, 1.000000000000000000, 0.8660254037844387076, 1.000000000000000000, 0.8660254037844387076, 1.000000000000000000, 0.8660254037844387076, 1.000000000000000000, 0.8660254037844387076, 1.000000000000000000, 0.8660254037844387076, 1.000000000000000000, 0.8660254037844387076, 1.000000000000000000, 0.8660254037844387076, 1.000000000000000000, 0.8660254037844387076, 1.000000000000000000, 0.8660254037844387076, 1.000000000000000000, 0.8660254037844387076, 1.000000000000000000, 0.8660254037844387076, 1.000000000000000000, 0.8660254037844387076, 1.000000000000000000, 0.8660254037844387076, 1.000000000000000000, 0.8660254037844387076, 1.000000000000000000, 0.8660254037844387076, 1.000000000000000000, 0.8660254037844387076, 1.000000000000000000, 0.8660254037844387076, 1.000000000000000000, 0.8660254037844387076, 1.000000000000000000, 0.8660254037844387076, 1.000000000000000000, 0.8660254037844387076, 1.000000000000000000, 0.8660254037844387076, 1.000000000000000000, 0.8660254037844387076, 1.000000000000000000, 0.8660254037844387076, 1.000000000000000000, 0.8660254037844387076, 1.000000000000000000, 0.8660254037844387076, 1.000000000000000000, 0.8660254037844387076, 1.000000000000000000, 0.8660254037844387076, 1.000000000000000000, 0.8660254037844387076, 1.000000000000000000, 0.8660254037844387076, 1.000000000000000000, 0.8660254037844387076, 1.000000000000000000, 0.8660254037844387076, 1.000000000000000000, 0.8660254037844387076, 1.000000000000000000, 0.8660254037844387076, 1.000000000000000000, 0.8660254037844387076, 1.000000000000000000, 0.8660254037844387076, 1.000000000000000000, 0.8660254037844387076, 1.000000000000000000, 0.8660254037844387076, 1.000000000000000000, 0.8660254037844387076, 1.000000000000000000, 0.8660254037844387076, 1.000000000000000000, 0.8660254037844387076, 1.000000000000000000, 0.8660254037844387076, 1.000000000000000000, 0.8660254037844387076, 1.000000000000000000, 0.8660254037844387076, 1.000000000000000000, 0.8660254037844387076, 1.000000000000000000, 0.8660254037844387076, 1.000000000000000000, 0.8660254037844387076, 1.000000000000000000, 0.8660254037844387076, 1.000000000000000000, 0.8660254037844387076, 1.000000000000000000, 0.8660254037844387076, 1.000000000000000000, 0.8660254037844387076, 1.000000000000000000, 0.8660254037844387076, 1.000000000000000000, 0.8660254037844387076, 1.000000000000000000, 0.8660254037844387076, 1.000000000000000000, 0.8660254037844387076, 1.000000000000000000, 0.8660254037844387076, 1.000000000000000000, 0.8660254037844387076, 1.000000000000000000, 0.8660254037844387076, 1.000000000000000000, 0.8660254037844387076, 1.000000000000000000, 0.8660254037844387076, 1.000000000000000000, 0.8660254037844387076, 1.000000000000000000, 0.8660254037844387076, 1.000000000000000000, 0.8660254037844387076, 1.000000000000000000, 0.8660254037844387076, 1.000000000000000000, 0.8660254037844387076, 1.000000000000000000, 0.8660254037844387076, 1.000000000000000000, 0.8660254037844387076, 1.000000000000000000, 0.8660254037844387076, 1.000000000000000000, 0.8660254037844387076, 1.000000000000000000, 0.8660254037844387076, 1.000000000000000000, 0.8660254037844387076, 1.000000000000000000, 0.8660254037844387076, 1.000000000000000000, 0.8660254037844387076, 1.000000000000000000, 0.8660254037844387076, 1.000000000000000000, 0.8660254037844387076, 1.000000000000000000, 0.8660254037844387076, 1.000000000000000000, 0.8660254037844387076, 1.000000000000000000, 0.8660254037844387076, 1.000000000000000000, 0.8660254037844387076, 1.000000000000000000, 0.8660254037844387076, 1.000000000000000000, 0.8660254037844387076, 1.000000000000000000, 0.8660254037844387076, 1.000000000000000000, 0.8660254037844387076, 1.000000000000000000, 0.8660254037844387076, 1.000000000000000000, 0.8660254037844387076, 1.000000000000000000, 0.8660254037844387076, 1.000000000000000000, 0.8660254037844387076, 1.000000000000000000, 0.8660254037844387076, 1.000000000000000000, 0.8660254037844387076, 1.000000000000000000, 0.8660254037844387076, 1.000000000000000000, 0.8660254037844387076, 1.000000000000000000, 0.8660254037844387076, 1.000000000000000000, 0.8660254037844387076, 1.000000000000000000, 0.8660254037844387076, 1.000000000000000000, 0.8660254037844387076, 1.000000000000000000, 0.8660254037844387076, 1.000000000000000000, 0.8660254037844387076, 1.000000000000000000, 0.8660254037844387076, 1.000000000000000000, 0.8660254037844387076, 1.000000000000000000, 0.8660254037844387076, 1.000000000000000000, 0.8660254037844387076, 1.000000000000000000, 0.8660254037844387076, 1.000000000000000000, 0.8660254037844387076, 1.000000000000000000, 0.8660254037844387076, 1.000000000000000000, 0.8660254037844387076, 1.000000000000000000, 0.8660254037844387076, 1.000000000000000000, 0.8660254037844387076, 1.000000000000000000, 0.8660254037844387076, 1.000000000000000000, 0.8660254037844387076, 1.000000000000000000, 0.8660254037844387076, 1.000000000000000000, 0.8660254037844387076, 1.000000000000000000, 0.8660254037844387076, 1.000000000000000000, 0.8660254037844387076, 1.000000000000000000, 0.8660254037844387076, 1.000000000000000000, 0.8660254037844387076, 1.000000000000000000, 0.8660254037844387076, 1.000000000000000000, 0.8660254037844387076, 1.000000000000000000, 0.8660254037844387076, 1.000000000000000000, 0.8660254037844387076, 1.000000000000000000, 0.8660254037844387076, 1.000000000000000000, 0.8660254037844387076, 1.000000000000000000, 0.8660254037844387076, 1.000000000000000000, 0.8660254037844387076, 1.000000000000000000, 0.8660254037844387076, 1.000000000000000000, 0.8660254037844387076, 1.000000000000000000, 0.8660254037844387076, 1.000000000000000000, 0.8660254037844387076, 1.000000000000000000, 0.8660254037844387076, 1.000000000000000000, 0.8660254037844387076, 1.000000000000000000, 0.8660254037844387076, 1.000000000000000000, 0.8660254037844387076, 1.000000000000000000, 0.8660254037844387076, 1.000000000000000000, 0.8660254037844387076, 1.000000000000000000, 0.8660254037844387076, 1.000000000000000000, 0.8660254037844387076, 1.000000000000000000, 0.8660254037844387076, 1.000000000000000000, 0.8660254037844387076, 1.000000000000000000, 0.8660254037844387076, 1.000000000000000000, 0.8660254037844387076, 1.000000000000000000, 0.8660254037844387076, 1.000000000000000000, 0.8660254037844387076, 1.000000000000000000, 0.8660254037844387076, 1.000000000000000000, 0.8660254037844387076, 1.000000000000000000, 0.8660254037844387076, 1.000000000000000000, 0.8660254037844387076, 1.000000000000000000, 0.8660254037844387076, 1.000000000000000000, 0.8660254037844387076, 1.000000000000000000, 0.8660254037844387076, 1.000000000000000000, 0.8660254037844387076, 1.000000000000000000, 0.8660254037844387076, 1.000000000000000000, 0.8660254037844387076, 1.000000000000000000, 0.8660254037844387076, 1.000000000000000000, 0.8660254037844387076, 1.000000000000000000, 0.8660254037844387076, 1.000000000000000000, 0.8660254037844387076, 1.000000000000000000, 0.8660254037844387076, 1.000000000000000000, 0.8660254037844387076, 1.000000000000000000, 0.8660254037844387076, 1.000000000000000000, 0.8660254037844387076, 1.000000000000000000, 0.8660254037844387076, 1.000000000000000000, 0.8660254037844387076, 1.000000000000000000, 0.8660254037844387076, 1.000000000000000000, 0.8660254037844387076, 1.000000000000000000, 0.8660254037844387076, 1.000000000000000000, 0.9548846395026606704, 0.9401540804572323662),
 ( 1.000000000000000000, 0.8660254037844387076, 1.000000000000000000, 0.8660254037844387076, 1.000000000000000000, 0.8660254037844387076, 1.000000000000000000, 0.8660254037844387076, 1.000000000000000000, 0.8660254037844387076, 1.000000000000000000, 0.8660254037844387076, 1.000000000000000000, 0.8660254037844387076, 1.000000000000000000, 0.8660254037844387076, 1.000000000000000000, 0.8660254037844387076, 1.000000000000000000, 0.8660254037844387076, 1.000000000000000000, 0.8660254037844387076, 1.000000000000000000, 0.8660254037844387076, 1.000000000000000000, 0.8660254037844387076, 1.000000000000000000, 0.8660254037844387076, 1.000000000000000000, 0.8660254037844387076, 1.000000000000000000, 0.8660254037844387076, 1.000000000000000000, 0.8660254037844387076, 1.000000000000000000, 0.8660254037844387076, 1.000000000000000000, 0.8660254037844387076, 1.000000000000000000, 0.8660254037844387076, 1.000000000000000000, 0.8660254037844387076, 1.000000000000000000, 0.8660254037844387076, 1.000000000000000000, 0.8660254037844387076, 1.000000000000000000, 0.8660254037844387076, 1.000000000000000000, 0.8660254037844387076, 1.000000000000000000, 0.8660254037844387076, 1.000000000000000000, 0.8660254037844387076, 1.000000000000000000, 0.8660254037844387076, 1.000000000000000000, 0.8660254037844387076, 1.000000000000000000, 0.8660254037844387076, 1.000000000000000000, 0.8660254037844387076, 1.000000000000000000, 0.8660254037844387076, 1.000000000000000000, 0.8660254037844387076, 1.000000000000000000, 0.8660254037844387076, 1.000000000000000000, 0.8660254037844387076, 1.000000000000000000, 0.8660254037844387076, 1.000000000000000000, 0.8660254037844387076, 1.000000000000000000, 0.8660254037844387076, 1.000000000000000000, 0.8660254037844387076, 1.000000000000000000, 0.8660254037844387076, 1.000000000000000000, 0.8660254037844387076, 1.000000000000000000, 0.8660254037844387076, 1.000000000000000000, 0.8660254037844387076, 1.000000000000000000, 0.8660254037844387076, 1.000000000000000000, 0.8660254037844387076, 1.000000000000000000, 0.8660254037844387076, 1.000000000000000000, 0.8660254037844387076, 1.000000000000000000, 0.8660254037844387076, 1.000000000000000000, 0.8660254037844387076, 1.000000000000000000, 0.8660254037844387076, 1.000000000000000000, 0.8660254037844387076, 1.000000000000000000, 0.8660254037844387076, 1.000000000000000000, 0.8660254037844387076, 1.000000000000000000, 0.8660254037844387076, 1.000000000000000000, 0.8660254037844387076, 1.000000000000000000, 0.8660254037844387076, 1.000000000000000000, 0.8660254037844387076, 1.000000000000000000, 0.8660254037844387076, 1.000000000000000000, 0.8660254037844387076, 1.000000000000000000, 0.8660254037844387076, 1.000000000000000000, 0.8660254037844387076, 1.000000000000000000, 0.8660254037844387076, 1.000000000000000000, 0.8660254037844387076, 1.000000000000000000, 0.8660254037844387076, 1.000000000000000000, 0.8660254037844387076, 1.000000000000000000, 0.8660254037844387076, 1.000000000000000000, 0.8660254037844387076, 1.000000000000000000, 0.8660254037844387076, 1.000000000000000000, 0.8660254037844387076, 1.000000000000000000, 0.8660254037844387076, 1.000000000000000000, 0.8660254037844387076, 1.000000000000000000, 0.8660254037844387076, 1.000000000000000000, 0.8660254037844387076, 1.000000000000000000, 0.8660254037844387076, 1.000000000000000000, 0.8660254037844387076, 1.000000000000000000, 0.8660254037844387076, 1.000000000000000000, 0.8660254037844387076, 1.000000000000000000, 0.8660254037844387076, 1.000000000000000000, 0.8660254037844387076, 1.000000000000000000, 0.8660254037844387076, 1.000000000000000000, 0.8660254037844387076, 1.000000000000000000, 0.8660254037844387076, 1.000000000000000000, 0.8660254037844387076, 1.000000000000000000, 0.8660254037844387076, 1.000000000000000000, 0.8660254037844387076, 1.000000000000000000, 0.8660254037844387076, 1.000000000000000000, 0.8660254037844387076, 1.000000000000000000, 0.8660254037844387076, 1.000000000000000000, 0.8660254037844387076, 1.000000000000000000, 0.8660254037844387076, 1.000000000000000000, 0.8660254037844387076, 1.000000000000000000, 0.8660254037844387076, 1.000000000000000000, 0.8660254037844387076, 1.000000000000000000, 0.8660254037844387076, 1.000000000000000000, 0.8660254037844387076, 1.000000000000000000, 0.8660254037844387076, 1.000000000000000000, 0.8660254037844387076, 1.000000000000000000, 0.8660254037844387076, 1.000000000000000000, 0.8660254037844387076, 1.000000000000000000, 0.8660254037844387076, 1.000000000000000000, 0.8660254037844387076, 1.000000000000000000, 0.8660254037844387076, 1.000000000000000000, 0.8660254037844387076, 1.000000000000000000, 0.8660254037844387076, 1.000000000000000000, 0.8660254037844387076, 1.000000000000000000, 0.8660254037844387076, 1.000000000000000000, 0.8660254037844387076, 1.000000000000000000, 0.8660254037844387076, 1.000000000000000000, 0.8660254037844387076, 1.000000000000000000, 0.8660254037844387076, 1.000000000000000000, 0.8660254037844387076, 1.000000000000000000, 0.8660254037844387076, 1.000000000000000000, 0.8660254037844387076, 1.000000000000000000, 0.8660254037844387076, 1.000000000000000000, 0.8660254037844387076, 1.000000000000000000, 0.8660254037844387076, 1.000000000000000000, 0.8660254037844387076, 1.000000000000000000, 0.8660254037844387076, 1.000000000000000000, 0.8660254037844387076, 1.000000000000000000, 0.8660254037844387076, 1.000000000000000000, 0.8660254037844387076, 1.000000000000000000, 0.8660254037844387076, 1.000000000000000000, 0.8660254037844387076, 1.000000000000000000, 0.8660254037844387076, 1.000000000000000000, 0.8660254037844387076, 1.000000000000000000, 0.8660254037844387076, 1.000000000000000000, 0.8660254037844387076, 1.000000000000000000, 0.8660254037844387076, 1.000000000000000000, 0.8660254037844387076, 1.000000000000000000, 0.8660254037844387076, 1.000000000000000000, 0.8660254037844387076, 1.000000000000000000, 0.8660254037844387076, 1.000000000000000000, 0.8660254037844387076, 1.000000000000000000, 0.8660254037844387076, 1.000000000000000000, 0.8660254037844387076, 1.000000000000000000, 0.8660254037844387076, 1.000000000000000000, 0.8660254037844387076, 1.000000000000000000, 0.8660254037844387076, 1.000000000000000000, 0.8660254037844387076, 1.000000000000000000, 0.8660254037844387076, 1.000000000000000000, 0.8660254037844387076, 1.000000000000000000, 0.8660254037844387076, 1.000000000000000000, 0.8660254037844387076, 1.000000000000000000, 0.8660254037844387076, 1.000000000000000000, 0.8660254037844387076, 1.000000000000000000, 0.8660254037844387076, 1.000000000000000000, 0.8660254037844387076, 1.000000000000000000, 0.8660254037844387076, 1.000000000000000000, 0.8660254037844387076, 1.000000000000000000, 0.8660254037844387076, 1.000000000000000000, 0.8660254037844387076, 1.000000000000000000, 0.8660254037844387076, 1.000000000000000000, 0.8660254037844387076, 1.000000000000000000, 0.8660254037844387076, 1.000000000000000000, 0.8660254037844387076, 1.000000000000000000, 0.8660254037844387076, 1.000000000000000000, 0.8660254037844387076, 1.000000000000000000, 0.8660254037844387076, 1.000000000000000000, 0.8660254037844387076, 1.000000000000000000, 0.8660254037844387076, 1.000000000000000000, 0.8660254037844387076, 1.000000000000000000, 0.8660254037844387076, 1.000000000000000000, 0.8660254037844387076, 1.000000000000000000, 0.8660254037844387076, 1.000000000000000000, 0.8660254037844387076, 1.000000000000000000, 0.8660254037844387076, 1.000000000000000000, 0.8660254037844387076, 1.000000000000000000, 0.8660254037844387076, 1.000000000000000000, 0.8660254037844387076, 1.000000000000000000, 0.8660254037844387076, 1.000000000000000000, 0.8660254037844387076, 1.000000000000000000, 0.8660254037844387076, 1.000000000000000000, 0.8660254037844387076, 1.000000000000000000, 0.9548846395026606704, 0.9401540804572323662) ) ) 
 REPRESENTATION_ITEM ( '' )  SURFACE ( )  );
#10002 = CARTESIAN_POINT ( 'NONE',  ( -7.385235650263080487, -10.35677961432909377, 5.003020502729047969 ) ) ;
#10003 = CARTESIAN_POINT ( 'NONE',  ( -4.243569643750000786, -23.09367458642858040, -8.699705261538101198 ) ) ;
#10004 = CIRCLE ( 'NONE', #12368, 10.00000000000000000 ) ;
#10005 = CARTESIAN_POINT ( 'NONE',  ( 3.607379964056306676, 28.99680007765648071, -2.690724712371305838 ) ) ;
#10006 = CARTESIAN_POINT ( 'NONE',  ( 1.071796769724485232, -23.30983881803475555, -2.034632595550943002 ) ) ;
#10007 = ORIENTED_EDGE ( 'NONE', *, *, #7265, .F. ) ;
#10008 = AXIS2_PLACEMENT_3D ( 'NONE', #11393, #17368, #12882 ) ;
#10009 = VERTEX_POINT ( 'NONE', #17866 ) ;
#10010 = CARTESIAN_POINT ( 'NONE',  ( 3.500000000000000444, 26.74680007765648071, -0.05647727720536935281 ) ) ;
#10011 = CARTESIAN_POINT ( 'NONE',  ( 4.898587196589417759E-16, -3.999999999999993339, 25.54267522293723758 ) ) ;
#10012 = CARTESIAN_POINT ( 'NONE',  ( -3.706921591972381904E-14, -18.25227819420489439, -8.759261836619732122 ) ) ;
#10013 = LINE ( 'NONE', #12441, #14469 ) ;
#10014 = EDGE_LOOP ( 'NONE', ( #11962, #14852, #6595, #10168 ) ) ;
#10015 = CARTESIAN_POINT ( 'NONE',  ( -2.115076519116425580, 17.37819992234354771, -3.012182706137062738 ) ) ;
#10016 = CARTESIAN_POINT ( 'NONE',  ( -2.121784821875005722, -25.28674396788038337, -5.424497759843593059 ) ) ;
#10017 = CARTESIAN_POINT ( 'NONE',  ( -2.500000000000001332, 15.49680007765647893, 0.05647727720535858364 ) ) ;
#10018 = CARTESIAN_POINT ( 'NONE',  ( 3.481649420246394122, 38.37819992234354771, 1.193696214020467439 ) ) ;
#10019 = FACE_OUTER_BOUND ( 'NONE', #8800, .T. ) ;
#10020 = DIRECTION ( 'NONE',  ( -1.000000000000000000, -0.000000000000000000, -0.000000000000000000 ) ) ;
#10021 = AXIS2_PLACEMENT_3D ( 'NONE', #3859, #17979, #14048 ) ;
#10022 = CARTESIAN_POINT ( 'NONE',  ( 2.121784821874994176, -26.30842699513068439, -6.883612338733362535 ) ) ;
#10023 = CYLINDRICAL_SURFACE ( 'NONE', #6131, 2.149999999999995470 ) ;
#10024 = CYLINDRICAL_SURFACE ( 'NONE', #12745, 4.000000000000000000 ) ;
#10025 = CARTESIAN_POINT ( 'NONE',  ( -3.000000000000001332, 15.00000000000000355, 3.048632113068340848E-14 ) ) ;
#10026 = CARTESIAN_POINT ( 'NONE',  ( 4.243569643750000786, -20.89974471738585748, -5.566448692132691001 ) ) ;
#10027 = CARTESIAN_POINT ( 'NONE',  ( -8.999999999999996447, -10.00000000000000000, 30.00000000000000000 ) ) ;
#10028 = DIRECTION ( 'NONE',  ( 0.000000000000000000, 0.000000000000000000, 1.000000000000000000 ) ) ;
#10029 = ORIENTED_EDGE ( 'NONE', *, *, #16027, .F. ) ;
#10030 = AXIS2_PLACEMENT_3D ( 'NONE', #1945, #8675, #1652 ) ;
#10031 = CARTESIAN_POINT ( 'NONE',  ( 2.500000000000001332, 23.25319992234354771, 0.05647727720530566764 ) ) ;
#10032 = CIRCLE ( 'NONE', #12995, 2.149999999999995470 ) ;
#10033 = LINE ( 'NONE', #41, #15749 ) ;
#10034 = CARTESIAN_POINT ( 'NONE',  ( -1.734723475976807094E-15, 16.59999999999999787, -2.500000000000000000 ) ) ;
#10035 = FACE_OUTER_BOUND ( 'NONE', #6182, .T. ) ;
#10036 = VERTEX_POINT ( 'NONE', #9485 ) ;
#10037 = CARTESIAN_POINT ( 'NONE',  ( -5.330712181944246111E-15, -23.97798589325759977, -1.419652468442682558 ) ) ;
#10038 = CARTESIAN_POINT ( 'NONE',  ( -0.05938372350927861171, 28.62180007765648071, -3.680117784833935701 ) ) ;
#10039 = CARTESIAN_POINT ( 'NONE',  ( 4.243569643749996345, -28.63886809700377611, -12.34757220902403851 ) ) ;
#10040 = CIRCLE ( 'NONE', #2391, 0.9999999999999991118 ) ;
#10041 = DIRECTION ( 'NONE',  ( -1.000000000000000000, 0.000000000000000000, 0.000000000000000000 ) ) ;
#10042 = CARTESIAN_POINT ( 'NONE',  ( 4.243569643749997233, -27.05794804431121037, -10.08978438695249480 ) ) ;
#10043 = CARTESIAN_POINT ( 'NONE',  ( 13.00000000000000178, 15.00000000000000178, 25.00000000000000355 ) ) ;
#10044 = DIRECTION ( 'NONE',  ( 0.000000000000000000, 0.000000000000000000, 1.000000000000000000 ) ) ;
#10045 = EDGE_CURVE ( 'NONE', #4093, #13916, #17687, .T. ) ;
#10046 = LINE ( 'NONE', #1456, #13541 ) ;
#10047 = CARTESIAN_POINT ( 'NONE',  ( 4.243569643749996345, -27.31605744066918007, -10.45840280688254431 ) ) ;
#10048 = CYLINDRICAL_SURFACE ( 'NONE', #9499, 4.000000000000000000 ) ;
#10049 = CARTESIAN_POINT ( 'NONE',  ( -4.000000000000000888, -20.69003083319747205, -5.266946226442914991 ) ) ;
#10050 = EDGE_CURVE ( 'NONE', #17559, #3748, #16282, .T. ) ;
#10051 = CARTESIAN_POINT ( 'NONE',  ( -0.8262555684461330152, 23.49680007765647716, -2.360188852285403982 ) ) ;
#10052 = VERTEX_POINT ( 'NONE', #17782 ) ;
#10053 = CARTESIAN_POINT ( 'NONE',  ( -3.481649420246370141, 25.37180007765647716, 1.193696214020542268 ) ) ;
#10054 = CARTESIAN_POINT ( 'NONE',  ( -1.999999999999996225, -20.99273590255452149, -11.73873072849375987 ) ) ;
#10055 = DIRECTION ( 'NONE',  ( 0.000000000000000000, 0.000000000000000000, 1.000000000000000000 ) ) ;
#10056 = CARTESIAN_POINT ( 'NONE',  ( -11.99999999999999822, 48.00000000000000000, 15.00000000000000000 ) ) ;
#10057 = MECHANICAL_DESIGN_GEOMETRIC_PRESENTATION_REPRESENTATION (  '', ( #18102 ), #17202 ) ;
#10058 = CARTESIAN_POINT ( 'NONE',  ( -2.481649420246391902, 37.12819992234354771, -0.8687765177875723666 ) ) ;
#10059 = VERTEX_POINT ( 'NONE', #10880 ) ;
#10060 = CARTESIAN_POINT ( 'NONE',  ( -2.121784821875005722, -27.64199220964684756, -8.788140841705278206 ) ) ;
#10061 = CARTESIAN_POINT ( 'NONE',  ( -1.444289557196047014, 35.99680007765647360, -4.262301884875704161 ) ) ;
#10062 = EDGE_CURVE ( 'NONE', #8139, #4992, #17602, .T. ) ;
#10063 = ORIENTED_EDGE ( 'NONE', *, *, #13044, .F. ) ;
#10064 = ADVANCED_FACE ( 'NONE', ( #10789 ), #15896, .T. ) ;
#10065 = FACE_OUTER_BOUND ( 'NONE', #7952, .T. ) ;
#10066 = VECTOR ( 'NONE', #1007, 1000.000000000000000 ) ;
#10067 = CARTESIAN_POINT ( 'NONE',  ( 3.157473464924626771, -21.86492304994214564, -2.325728555794866814 ) ) ;
#10068 = CARTESIAN_POINT ( 'NONE',  ( 3.579096709490575479E-14, -23.83758431146952361, -2.788331270066955359 ) ) ;
#10069 = CARTESIAN_POINT ( 'NONE',  ( 2.121784821874994176, -24.24355182426693389, -3.934664979292979314 ) ) ;
#10070 = ORIENTED_EDGE ( 'NONE', *, *, #16822, .T. ) ;
#10071 = APPLICATION_CONTEXT ( 'automotive_design' ) ;
#10072 = CARTESIAN_POINT ( 'NONE',  ( 8.673617379884035472E-15, 13.00000000000000178, -6.999999999999996447 ) ) ;
#10073 = ORIENTED_EDGE ( 'NONE', *, *, #2210, .T. ) ;
#10074 = ORIENTED_EDGE ( 'NONE', *, *, #12523, .T. ) ;
#10075 = LINE ( 'NONE', #3054, #13388 ) ;
#10076 = CARTESIAN_POINT ( 'NONE',  ( 3.999999999999993339, 0.000000000000000000, 30.00000000000000000 ) ) ;
#10077 = CARTESIAN_POINT ( 'NONE',  ( -3.607379964056363075, 14.75319992234354416, -2.690724712371229899 ) ) ;
#10078 = CARTESIAN_POINT ( 'NONE',  ( 3.500000000000000444, 30.75319992234354416, 0.05647727720529520379 ) ) ;
#10079 = CARTESIAN_POINT ( 'NONE',  ( 1.989345975306426206, 36.49680007765648071, -1.515154207786343799 ) ) ;
#10080 = EDGE_CURVE ( 'NONE', #13037, #12310, #5229, .T. ) ;
#10081 = ORIENTED_EDGE ( 'NONE', *, *, #15287, .T. ) ;
#10082 = CARTESIAN_POINT ( 'NONE',  ( 4.518350579753602325, 33.12819992234354771, -1.405661355842793725 ) ) ;
#10083 = CARTESIAN_POINT ( 'NONE',  ( 3.999999999999996447, -24.73269308191887461, -7.014148351807475201 ) ) ;
#10084 = EDGE_LOOP ( 'NONE', ( #3786, #7719, #17961, #1133 ) ) ;
#10085 = DIRECTION ( 'NONE',  ( -0.000000000000000000, -0.5735764363510414965, -0.8191520442889950182 ) ) ;
#10086 = CARTESIAN_POINT ( 'NONE',  ( 1.027846397803542144, 28.74680007765647716, -3.346150245485522312 ) ) ;
#10087 = CARTESIAN_POINT ( 'NONE',  ( 10.00265829479232060, -9.915630618149643638, 6.507612919863985823 ) ) ;
#10088 = CARTESIAN_POINT ( 'NONE',  ( -4.243569643750004339, -24.04667175346823527, -5.789236154435278614 ) ) ;
#10089 = CARTESIAN_POINT ( 'NONE',  ( -4.518350579753632523, 28.12180007765647716, -1.405661355842698468 ) ) ;
#10090 = CARTESIAN_POINT ( 'NONE',  ( 2.000000000000004441, -17.09958584011689098, -6.178736226875440884 ) ) ;
#10091 = EDGE_LOOP ( 'NONE', ( #12437, #5540, #5402, #6518 ) ) ;
#10092 = VERTEX_POINT ( 'NONE', #11906 ) ;
#10093 = CARTESIAN_POINT ( 'NONE',  ( -2.864755990943265829, 20.74680007765647716, -2.011557305968488141 ) ) ;
#10094 = PLANE ( 'NONE',  #3916 ) ;
#10095 = PRESENTATION_STYLE_ASSIGNMENT (( #5579 ) ) ;
#10096 = CARTESIAN_POINT ( 'NONE',  ( 1.071796769724504328, -24.40680375326105533, -3.601260881260418767 ) ) ;
#10097 = CARTESIAN_POINT ( 'NONE',  ( -1.999999999999996225, -23.76741191269774234, -15.70137874173500947 ) ) ;
#10098 = ORIENTED_EDGE ( 'NONE', *, *, #18188, .T. ) ;
#10099 = CARTESIAN_POINT ( 'NONE',  ( -1.135272562821019626, 16.50319992234354416, 3.311245368580577164 ) ) ;
#10100 = CARTESIAN_POINT ( 'NONE',  ( 4.000000000000003553, -23.80990433270476458, -13.74890525313040612 ) ) ;
#10101 = CARTESIAN_POINT ( 'NONE',  ( 4.243569643749996345, -25.50929166616339572, -7.878073867372210159 ) ) ;
#10102 = CARTESIAN_POINT ( 'NONE',  ( -1.027846397803541700, 39.99680007765648071, 3.346150245485522312 ) ) ;
#10103 = ADVANCED_FACE ( 'NONE', ( #5226 ), #2281, .F. ) ;
#10104 = CIRCLE ( 'NONE', #1550, 2.149999999999995470 ) ;
#10105 = CARTESIAN_POINT ( 'NONE',  ( -2.798362969681409851, 32.25319992234354771, -2.102939460078765421 ) ) ;
#10106 = AXIS2_PLACEMENT_3D ( 'NONE', #4938, #2182, #10594 ) ;
#10107 = DIRECTION ( 'NONE',  ( -0.000000000000000000, -1.000000000000000000, -0.000000000000000000 ) ) ;
#10108 = ADVANCED_FACE ( 'NONE', ( #13757, #16461, #2195, #6438, #4865, #2103 ), #14981, .F. ) ;
#10109 = FACE_OUTER_BOUND ( 'NONE', #6680, .T. ) ;
#10110 =( BOUNDED_CURVE ( )  B_SPLINE_CURVE ( 3, ( #1180, #5432, #11078, #6726 ),
 .UNSPECIFIED., .F., .F. ) 
 B_SPLINE_CURVE_WITH_KNOTS ( ( 4, 4 ),
 ( 3.141592653589793116, 4.171289454427542509 ),
 .UNSPECIFIED. ) 
 CURVE ( )  GEOMETRIC_REPRESENTATION_ITEM ( )  RATIONAL_B_SPLINE_CURVE ( ( 1.000000000000000000, 0.9135782535825738293, 0.9135782535825738293, 1.000000000000000000 ) ) 
 REPRESENTATION_ITEM ( '' )  );
#10111 = CARTESIAN_POINT ( 'NONE',  ( -2.121784821874996396, -20.15854069044762298, -10.91513480593371987 ) ) ;
#10112 = CARTESIAN_POINT ( 'NONE',  ( -6.428571428571423496, -11.73421655796351892, 14.25837509840161310 ) ) ;
#10113 = DIRECTION ( 'NONE',  ( -0.000000000000000000, -1.000000000000000000, -0.000000000000000000 ) ) ;
#10114 = VECTOR ( 'NONE', #16293, 1000.000000000000000 ) ;
#10115 = FACE_OUTER_BOUND ( 'NONE', #7320, .T. ) ;
#10116 = CIRCLE ( 'NONE', #5090, 0.9999999999999991118 ) ;
#10117 = CYLINDRICAL_SURFACE ( 'NONE', #6461, 4.000000000000000000 ) ;
#10118 = CARTESIAN_POINT ( 'NONE',  ( 4.730628863548789710E-15, -16.04700144155306774, -7.178993278803624811 ) ) ;
#10119 = CARTESIAN_POINT ( 'NONE',  ( -1.643582917929414133, 15.00000000000000711, -2.763362831372398798 ) ) ;
#10120 = CARTESIAN_POINT ( 'NONE',  ( -5.577813053751546416E-15, -23.90211166126395881, -2.880485876056233518 ) ) ;
#10121 = ORIENTED_EDGE ( 'NONE', *, *, #4978, .F. ) ;
#10122 = CARTESIAN_POINT ( 'NONE',  ( 0.7188294034286553114, 18.75319992234354416, 2.395093729190349130 ) ) ;
#10123 = AXIS2_PLACEMENT_3D ( 'NONE', #17430, #10534, #13223 ) ;
#10124 = CARTESIAN_POINT ( 'NONE',  ( -3.999999999999997335, -20.30391836480407619, -8.741838381407161407 ) ) ;
#10125 = LINE ( 'NONE', #8926, #7452 ) ;
#10126 = CARTESIAN_POINT ( 'NONE',  ( 4.481649420246366589, 19.12180007765647360, -1.518615910253458212 ) ) ;
#10127 = CARTESIAN_POINT ( 'NONE',  ( -1.734723475976807094E-15, 27.59999999999999432, -2.500000000000000000 ) ) ;
#10128 = ORIENTED_EDGE ( 'NONE', *, *, #62, .T. ) ;
#10129 = VECTOR ( 'NONE', #942, 1000.000000000000000 ) ;
#10130 = CARTESIAN_POINT ( 'NONE',  ( -2.121784821875005722, -22.73791367884544812, -1.784390863034371666 ) ) ;
#10131 = CARTESIAN_POINT ( 'NONE',  ( -0.05938372350927861171, 33.62180007765648071, -3.680117784833935701 ) ) ;
#10132 = CIRCLE ( 'NONE', #2754, 0.9999999999999991118 ) ;
#10133 = CARTESIAN_POINT ( 'NONE',  ( -5.279047395330986450E-15, -23.82825856781747831, -1.696164096186225656 ) ) ;
#10134 = CARTESIAN_POINT ( 'NONE',  ( -13.00000000000000178, 15.00000000000000178, -25.00000000000000355 ) ) ;
#10135 = CARTESIAN_POINT ( 'NONE',  ( -4.243569643750004339, -27.14398450976385746, -10.21265719359585056 ) ) ;
#10136 = CARTESIAN_POINT ( 'NONE',  ( 0.000000000000000000, 9.254131787996968228, 30.52396275209373044 ) ) ;
#10137 = CARTESIAN_POINT ( 'NONE',  ( 0.000000000000000000, 3.000000000000000000, 0.000000000000000000 ) ) ;
#10138 = DIRECTION ( 'NONE',  ( 1.000000000000000000, 0.000000000000000000, 0.000000000000000000 ) ) ;
#10139 = CARTESIAN_POINT ( 'NONE',  ( -2.121784821874996396, -21.41682399769271328, -12.71214960309270303 ) ) ;
#10140 = CARTESIAN_POINT ( 'NONE',  ( -8.500000000000010658, 15.00000000000000178, 18.34999999999999432 ) ) ;
#10141 = VECTOR ( 'NONE', #4966, 1000.000000000000000 ) ;
#10142 = CARTESIAN_POINT ( 'NONE',  ( -3.999999999999997335, -18.56167994009273059, -6.253664047886104527 ) ) ;
#10143 = AXIS2_PLACEMENT_3D ( 'NONE', #6758, #2521, #3709 ) ;
#10144 = EDGE_CURVE ( 'NONE', #4809, #10036, #15438, .T. ) ;
#10145 = CARTESIAN_POINT ( 'NONE',  ( -1.593127413382998459, 23.37180007765648071, -2.091722143975139669 ) ) ;
#10146 = ORIENTED_EDGE ( 'NONE', *, *, #4781, .F. ) ;
#10147 = CARTESIAN_POINT ( 'NONE',  ( -3.500000000000000444, 22.99680007765647716, 0.05647727720536892260 ) ) ;
#10148 = FACE_OUTER_BOUND ( 'NONE', #6070, .T. ) ;
#10149 = FILL_AREA_STYLE_COLOUR ( '', #7752 ) ;
#10150 = CARTESIAN_POINT ( 'NONE',  ( -2.000000000000005773, -25.80762308735776145, -6.536148542923068128 ) ) ;
#10151 = CARTESIAN_POINT ( 'NONE',  ( -1.593127413382952939, 39.12819992234354771, 2.091722143975172532 ) ) ;
#10152 = EDGE_CURVE ( 'NONE', #1108, #10845, #4338, .T. ) ;
#10153 = ORIENTED_EDGE ( 'NONE', *, *, #5808, .T. ) ;
#10154 = CARTESIAN_POINT ( 'NONE',  ( 4.243569643750003451, -22.00086816302836823, -11.41050605784547578 ) ) ;
#10155 = CARTESIAN_POINT ( 'NONE',  ( -2.829195390882805139, 35.87180007765647360, -3.793023760679206102 ) ) ;
#10156 = EDGE_CURVE ( 'NONE', #4808, #10864, #17994, .T. ) ;
#10157 = ORIENTED_EDGE ( 'NONE', *, *, #12270, .T. ) ;
#10158 = AXIS2_PLACEMENT_3D ( 'NONE', #15452, #12741, #1715 ) ;
#10159 = PLANE ( 'NONE',  #5327 ) ;
#10160 = DIRECTION ( 'NONE',  ( -1.000000000000000000, -0.000000000000000000, -0.000000000000000000 ) ) ;
#10161 = CARTESIAN_POINT ( 'NONE',  ( 4.243569643750000786, -25.57797752637403832, -12.24765755336480666 ) ) ;
#10162 = CARTESIAN_POINT ( 'NONE',  ( 3.999999999999996447, -23.95836489284496906, -5.908293092017329329 ) ) ;
#10163 = DIRECTION ( 'NONE',  ( -0.000000000000000000, 1.000000000000000000, -0.000000000000000000 ) ) ;
#10164 = CARTESIAN_POINT ( 'NONE',  ( 1.071796769724504328, -25.89093278161442768, -5.720816794851426579 ) ) ;
#10165 = CARTESIAN_POINT ( 'NONE',  ( -2.121784821874996396, -18.60988431229980833, -8.703424286353433459 ) ) ;
#10166 = ORIENTED_EDGE ( 'NONE', *, *, #11440, .F. ) ;
#10167 = CYLINDRICAL_SURFACE ( 'NONE', #18320, 0.9999999999999991118 ) ;
#10168 = ORIENTED_EDGE ( 'NONE', *, *, #8265, .F. ) ;
#10169 = ORIENTED_EDGE ( 'NONE', *, *, #4750, .F. ) ;
#10170 = DIRECTION ( 'NONE',  ( 0.000000000000000000, 0.000000000000000000, -1.000000000000000000 ) ) ;
#10171 = CARTESIAN_POINT ( 'NONE',  ( 3.061616997868382648E-16, 5.000000000000000000, -2.499999999999999556 ) ) ;
#10172 =( LENGTH_UNIT ( ) NAMED_UNIT ( * ) SI_UNIT ( .MILLI., .METRE. ) );
#10173 = CARTESIAN_POINT ( 'NONE',  ( 1.444289557195957086, 22.75319992234354061, -4.262301884875733471 ) ) ;
#10174 = CARTESIAN_POINT ( 'NONE',  ( 1.135272562821020070, 27.75319992234354416, -3.311245368580577164 ) ) ;
#10175 = CARTESIAN_POINT ( 'NONE',  ( 2.481649420246374138, 39.12180007765647360, -0.8687765177876252132 ) ) ;
#10176 = EDGE_CURVE ( 'NONE', #4921, #4547, #11150, .T. ) ;
#10177 = ORIENTED_EDGE ( 'NONE', *, *, #14142, .T. ) ;
#10178 = CARTESIAN_POINT ( 'NONE',  ( -4.499999999999999112, 37.00319992234354771, -0.05647727720528529505 ) ) ;
#10179 = EDGE_CURVE ( 'NONE', #13163, #7853, #13659, .T. ) ;
#10180 = CARTESIAN_POINT ( 'NONE',  ( -1.999999999999996225, -21.18631794911805599, -12.01519454243453211 ) ) ;
#10181 = ORIENTED_EDGE ( 'NONE', *, *, #17408, .T. ) ;
#10182 = CARTESIAN_POINT ( 'NONE',  ( 8.499999999999994671, 13.00000000000000000, 20.49999999999999645 ) ) ;
#10183 = CARTESIAN_POINT ( 'NONE',  ( 2.798362969681366330, 33.99680007765648071, -2.102939460078824929 ) ) ;
#10184 = CARTESIAN_POINT ( 'NONE',  ( -9.997135785739454050, -9.916563802935840499, 4.936593098934934254 ) ) ;
#10185 = CARTESIAN_POINT ( 'NONE',  ( 2.121784821875004390, -18.10442007776545736, -7.981546547323755014 ) ) ;
#10186 = CARTESIAN_POINT ( 'NONE',  ( 1.444289557196047680, 29.74680007765648071, 4.262301884875704161 ) ) ;
#10187 = CARTESIAN_POINT ( 'NONE',  ( 3.250767888004682415, -21.90484815091188509, -2.246271217071878823 ) ) ;
#10188 = ORIENTED_EDGE ( 'NONE', *, *, #15907, .F. ) ;
#10189 = ORIENTED_EDGE ( 'NONE', *, *, #11841, .T. ) ;
#10190 = CARTESIAN_POINT ( 'NONE',  ( -2.211161402132902243, 28.37180007765647716, -2.942372952327172886 ) ) ;
#10191 =( NAMED_UNIT ( * ) SI_UNIT ( $, .STERADIAN. ) SOLID_ANGLE_UNIT ( ) );
#10192 = DIRECTION ( 'NONE',  ( -0.000000000000000000, -0.5735764363510414965, -0.8191520442889950182 ) ) ;
#10193 = CARTESIAN_POINT ( 'NONE',  ( 1.999999999999994449, -27.76495267570075143, -9.331504893052493088 ) ) ;
#10194 = VERTEX_POINT ( 'NONE', #10607 ) ;
#10195 = CARTESIAN_POINT ( 'NONE',  ( 2.211161402132839626, 17.87819992234354771, -2.942372952327218183 ) ) ;
#10196 = DIRECTION ( 'NONE',  ( 0.000000000000000000, 0.000000000000000000, 1.000000000000000000 ) ) ;
#10197 = CARTESIAN_POINT ( 'NONE',  ( -2.121784821874996396, -18.57762063775506078, -8.657346983862177936 ) ) ;
#10198 = CARTESIAN_POINT ( 'NONE',  ( -2.055738996568313048, 15.74680007765648071, -1.423772053676023441 ) ) ;
#10199 = CARTESIAN_POINT ( 'NONE',  ( -3.518350579753605434, 31.87819992234354416, 1.080741659609877781 ) ) ;
#10200 = CARTESIAN_POINT ( 'NONE',  ( -2.121784821875005722, -29.96497677686856775, -12.10570662107570961 ) ) ;
#10201 = DIRECTION ( 'NONE',  ( -3.469446951953613696E-16, -0.000000000000000000, -1.000000000000000000 ) ) ;
#10202 = CARTESIAN_POINT ( 'NONE',  ( 2.121784821875004390, -19.68534013045801956, -10.23933436939529606 ) ) ;
#10203 = DIRECTION ( 'NONE',  ( 3.469446951953612217E-16, -0.000000000000000000, 1.000000000000000000 ) ) ;
#10204 = CARTESIAN_POINT ( 'NONE',  ( -5.002737418184070251, -14.83391033323086994, -6.661572473864194599 ) ) ;
#10205 = EDGE_CURVE ( 'NONE', #3333, #6382, #13220, .T. ) ;
#10206 = LINE ( 'NONE', #4653, #12443 ) ;
#10207 = EDGE_CURVE ( 'NONE', #13916, #5047, #13478, .T. ) ;
#10208 = CARTESIAN_POINT ( 'NONE',  ( 4.000000000000000000, -1.759474945355381292, 3.047500000000002540 ) ) ;
#10209 = ORIENTED_EDGE ( 'NONE', *, *, #6272, .F. ) ;
#10210 = EDGE_LOOP ( 'NONE', ( #12601, #15209, #5934, #17265 ) ) ;
#10211 = CARTESIAN_POINT ( 'NONE',  ( 2.121784821875004390, -17.84631068140748766, -7.612928127393706390 ) ) ;
#10212 = DIRECTION ( 'NONE',  ( 0.000000000000000000, 0.000000000000000000, 1.000000000000000000 ) ) ;
#10213 = CYLINDRICAL_SURFACE ( 'NONE', #14148, 4.000000000000001776 ) ;
#10214 = EDGE_CURVE ( 'NONE', #1959, #9924, #2298, .T. ) ;
#10215 = ORIENTED_EDGE ( 'NONE', *, *, #10971, .F. ) ;
#10216 = CARTESIAN_POINT ( 'NONE',  ( 1.497042530366522461, 23.62819992234354416, 2.161531897785029965 ) ) ;
#10217 = CARTESIAN_POINT ( 'NONE',  ( -4.243569643749997233, -24.97988077932658513, -15.66497698787144977 ) ) ;
#10218 = CARTESIAN_POINT ( 'NONE',  ( -3.500000000000000444, 15.49680007765647893, 0.05647727720536892260 ) ) ;
#10219 = VECTOR ( 'NONE', #11321, 1000.000000000000000 ) ;
#10220 = EDGE_CURVE ( 'NONE', #5429, #11926, #12920, .T. ) ;
#10221 = DIRECTION ( 'NONE',  ( 0.000000000000000000, 0.000000000000000000, 1.000000000000000000 ) ) ;
#10222 = CARTESIAN_POINT ( 'NONE',  ( -1.734723475976807094E-15, 23.19999999999999574, -2.500000000000000000 ) ) ;
#10223 = ORIENTED_EDGE ( 'NONE', *, *, #375, .F. ) ;
#10224 = CARTESIAN_POINT ( 'NONE',  ( 2.864755990943265829, 39.49680007765647360, 2.011557305968487697 ) ) ;
#10225 = CARTESIAN_POINT ( 'NONE',  ( 4.730628863548789710E-15, -22.53200002504703647, -16.44053107954607640 ) ) ;
#10226 = AXIS2_PLACEMENT_3D ( 'NONE', #7844, #18069, #15091 ) ;
#10227 = CARTESIAN_POINT ( 'NONE',  ( 1.533898589781675205E-14, -28.28997139934942595, -9.146999014867043698 ) ) ;
#10228 = CARTESIAN_POINT ( 'NONE',  ( 2.121784821875004390, -22.75038921220889065, -14.61667810606461337 ) ) ;
#10229 = AXIS2_PLACEMENT_3D ( 'NONE', #16643, #3915, #5577 ) ;
#10230 = FACE_OUTER_BOUND ( 'NONE', #6477, .T. ) ;
#10231 = PRODUCT_RELATED_PRODUCT_CATEGORY ( 'part', '', ( #8117 ) ) ;
#10232 = DIRECTION ( 'NONE',  ( 0.000000000000000000, 0.8660254037844385966, 0.5000000000000003331 ) ) ;
#10233 = CARTESIAN_POINT ( 'NONE',  ( 1.300000000000000044, 1.082531754730549300, 0.6250000000000008882 ) ) ;
#10234 = TOROIDAL_SURFACE ( 'NONE', #10830, 4.400000000000002132, 0.4000000000000000222 ) ;
#10235 = CARTESIAN_POINT ( 'NONE',  ( -5.330712181944245322E-15, -28.84980074951425877, -8.377325144622332687 ) ) ;
#10236 = CARTESIAN_POINT ( 'NONE',  ( 15.00000000000000355, -4.000000000000000000, -30.00000000000000000 ) ) ;
#10237 = CARTESIAN_POINT ( 'NONE',  ( 4.713407268011036227E-15, -16.71294755970913215, -7.639718490920175853 ) ) ;
#10238 = CARTESIAN_POINT ( 'NONE',  ( -0.05938372350926768989, 26.12180007765648426, -2.628655560595669183 ) ) ;
#10239 = VERTEX_POINT ( 'NONE', #2909 ) ;
#10240 = CARTESIAN_POINT ( 'NONE',  ( 1.135272562821090458, 19.74680007765648071, 3.311245368580554072 ) ) ;
#10241 = FACE_OUTER_BOUND ( 'NONE', #16884, .T. ) ;
#10242 = DIRECTION ( 'NONE',  ( 0.000000000000000000, 0.000000000000000000, 1.000000000000000000 ) ) ;
#10243 = CARTESIAN_POINT ( 'NONE',  ( 2.000000000000004441, -22.84251990978664182, -14.38049607132576746 ) ) ;
#10244 = CARTESIAN_POINT ( 'NONE',  ( 13.00000000000000178, 48.00000000000000000, 16.00000000000000000 ) ) ;
#10245 = CARTESIAN_POINT ( 'NONE',  ( -2.864755990943222308, 19.25319992234354416, 2.011557305968548093 ) ) ;
#10246 = ORIENTED_EDGE ( 'NONE', *, *, #13173, .F. ) ;
#10247 = CARTESIAN_POINT ( 'NONE',  ( 4.243569643750000786, -24.28743054458419692, -10.40456545371456620 ) ) ;
#10248 = CARTESIAN_POINT ( 'NONE',  ( 0.05938372350927906274, 17.37180007765647005, 3.680117784833935701 ) ) ;
#10249 = TOROIDAL_SURFACE ( 'NONE', #2575, 9.000000000000001776, 0.9999999999999991118 ) ;
#10250 = ORIENTED_EDGE ( 'NONE', *, *, #5297, .T. ) ;
#10251 = PRESENTATION_STYLE_ASSIGNMENT (( #5991 ) ) ;
#10252 = CARTESIAN_POINT ( 'NONE',  ( 0.000000000000000000, 38.59999999999999432, 2.500000000000000000 ) ) ;
#10253 = CARTESIAN_POINT ( 'NONE',  ( 4.243569643750000786, -25.06175873365810247, -11.51042071350471119 ) ) ;
#10254 = DIRECTION ( 'NONE',  ( -1.000000000000000000, 0.000000000000000000, 0.000000000000000000 ) ) ;
#10255 = DIRECTION ( 'NONE',  ( 0.6985514936319299206, -0.7155597883787208069, 0.000000000000000000 ) ) ;
#10256 = DIRECTION ( 'NONE',  ( 0.000000000000000000, 0.000000000000000000, -1.000000000000000000 ) ) ;
#10257 = CARTESIAN_POINT ( 'NONE',  ( -4.243569643750000786, -21.83539127918348299, -6.902690464379118040 ) ) ;
#10258 = ORIENTED_EDGE ( 'NONE', *, *, #1512, .T. ) ;
#10259 = DIRECTION ( 'NONE',  ( 0.000000000000000000, 0.000000000000000000, 1.000000000000000000 ) ) ;
#10260 = DIRECTION ( 'NONE',  ( 0.000000000000000000, 0.000000000000000000, -1.000000000000000000 ) ) ;
#10261 = ORIENTED_EDGE ( 'NONE', *, *, #4731, .T. ) ;
#10262 = AXIS2_PLACEMENT_3D ( 'NONE', #10771, #2265, #6509 ) ;
#10263 = ORIENTED_EDGE ( 'NONE', *, *, #9214, .T. ) ;
#10264 = CARTESIAN_POINT ( 'NONE',  ( -8.500000000000010658, 13.00000000000000000, 18.34999999999999432 ) ) ;
#10265 = ADVANCED_FACE ( 'NONE', ( #16839 ), #14419, .T. ) ;
#10266 = DIRECTION ( 'NONE',  ( 3.469446951953612217E-16, -0.000000000000000000, 1.000000000000000000 ) ) ;
#10267 = CARTESIAN_POINT ( 'NONE',  ( 1.336863392178569754, 23.75319992234354771, 4.297206761780648421 ) ) ;
#10268 = CARTESIAN_POINT ( 'NONE',  ( -1.135272562821019626, 31.50319992234354416, 3.311245368580577164 ) ) ;
#10269 = CARTESIAN_POINT ( 'NONE',  ( 2.500000000000001332, 23.25319992234354771, 0.05647727720530566764 ) ) ;
#10270 = ORIENTED_EDGE ( 'NONE', *, *, #12450, .T. ) ;
#10271 = CARTESIAN_POINT ( 'NONE',  ( -4.518350579753602325, 31.87819992234354416, 1.405661355842794391 ) ) ;
#10272 = CARTESIAN_POINT ( 'NONE',  ( 4.713407268011036227E-15, -17.68085779534656510, -9.022037564651093078 ) ) ;
#10273 = ORIENTED_EDGE ( 'NONE', *, *, #14901, .F. ) ;
#10274 = VECTOR ( 'NONE', #2866, 1000.000000000000000 ) ;
#10275 = CARTESIAN_POINT ( 'NONE',  ( -11.99999999999999822, 13.00000000000000178, 15.00000000000000000 ) ) ;
#10276 = CIRCLE ( 'NONE', #16829, 2.000000000000001776 ) ;
#10277 = CARTESIAN_POINT ( 'NONE',  ( -2.798362969681365886, 32.74680007765648071, 2.102939460078824929 ) ) ;
#10278 = CARTESIAN_POINT ( 'NONE',  ( -7.256038713980983879, -10.36824963302216318, 4.264491367891564799 ) ) ;
#10279 = CARTESIAN_POINT ( 'NONE',  ( 4.243569643750000786, -21.93218230281772918, -7.040922371852881945 ) ) ;
#10280 = CARTESIAN_POINT ( 'NONE',  ( -4.481649420246366589, 27.87180007765647716, 1.518615910253458878 ) ) ;
#10281 = CARTESIAN_POINT ( 'NONE',  ( -15.00000000000000178, 13.00000000000000178, 24.99999999999999645 ) ) ;
#10282 = ADVANCED_FACE ( 'NONE', ( #16746 ), #15346, .T. ) ;
#10283 = ORIENTED_EDGE ( 'NONE', *, *, #3332, .F. ) ;
#10284 = CARTESIAN_POINT ( 'NONE',  ( -2.115076519116362519, 32.62180007765646650, 3.012182706137107147 ) ) ;
#10285 = CLOSED_SHELL ( 'NONE', ( #13280, #7334, #3834, #15791, #6268, #7840, #12471, #5681, #6039, #6719 ) ) ;
#10286 = CARTESIAN_POINT ( 'NONE',  ( 0.000000000000000000, 29.79999999999999716, 2.500000000000000000 ) ) ;
#10287 = FACE_OUTER_BOUND ( 'NONE', #7088, .T. ) ;
#10288 = DIRECTION ( 'NONE',  ( 0.000000000000000000, -0.000000000000000000, 1.000000000000000000 ) ) ;
#10289 = CARTESIAN_POINT ( 'NONE',  ( -1.071796769724494114, -29.78562712842163762, -11.28301676311397017 ) ) ;
#10290 = ORIENTED_EDGE ( 'NONE', *, *, #11021, .F. ) ;
#10291 = AXIS2_PLACEMENT_3D ( 'NONE', #15429, #2727, #14020 ) ;
#10292 = CARTESIAN_POINT ( 'NONE',  ( 2.115076519116426024, 23.62819992234354416, 3.012182706137062294 ) ) ;
#10293 = CARTESIAN_POINT ( 'NONE',  ( 8.500000000000019540, 0.000000000000000000, -18.49999999999998934 ) ) ;
#10294 = TOROIDAL_SURFACE ( 'NONE', #9408, 2.200000000000000178, 0.2000000000000000111 ) ;
#10295 = CARTESIAN_POINT ( 'NONE',  ( -5.330712181944245322E-15, -26.01059738957660272, -4.322522525391808479 ) ) ;
#10296 = CARTESIAN_POINT ( 'NONE',  ( -1.497042530366477164, 22.62180007765647716, 2.161531897785062384 ) ) ;
#10297 = CARTESIAN_POINT ( 'NONE',  ( -3.481649420246394122, 32.12819992234353350, -1.193696214020467883 ) ) ;
#10298 = CARTESIAN_POINT ( 'NONE',  ( 2.121784821874994176, -29.66384914778427628, -11.67565179782398310 ) ) ;
#10299 = CARTESIAN_POINT ( 'NONE',  ( -4.000000000000004441, -28.43226109638308330, -12.29767903747149660 ) ) ;
#10300 = CARTESIAN_POINT ( 'NONE',  ( 2.121784821874994176, -25.27598940969881269, -5.409138659013170702 ) ) ;
#10301 = DIRECTION ( 'NONE',  ( 0.000000000000000000, 0.000000000000000000, 1.000000000000000000 ) ) ;
#10302 = AXIS2_PLACEMENT_3D ( 'NONE', #11414, #15262, #2558 ) ;
#10303 = CARTESIAN_POINT ( 'NONE',  ( 1.743066579297358403E-15, -23.41446612136426708, -16.13163023522068684 ) ) ;
#10304 = CARTESIAN_POINT ( 'NONE',  ( -2.000000000000005773, -23.48463852013604480, -3.218582763552638948 ) ) ;
#10305 = CARTESIAN_POINT ( 'NONE',  ( -1.734723475976807094E-15, 31.99999999999999289, -2.500000000000000000 ) ) ;
#10306 = EDGE_LOOP ( 'NONE', ( #3994, #1422, #13152, #15596 ) ) ;
#10307 = VERTEX_POINT ( 'NONE', #17019 ) ;
#10308 = CARTESIAN_POINT ( 'NONE',  ( -4.000000000000004441, -21.52783474451236145, -2.437136305349486332 ) ) ;
#10309 = CARTESIAN_POINT ( 'NONE',  ( 8.000000000000000000, 13.00000000000000178, 2.500000000000000000 ) ) ;
#10310 = CARTESIAN_POINT ( 'NONE',  ( 9.000000000000001776, 38.59999999999999432, -2.500000000000002665 ) ) ;
#10311 = VERTEX_POINT ( 'NONE', #9937 ) ;
#10312 = CARTESIAN_POINT ( 'NONE',  ( -1.989345975306457071, 29.75319992234354771, -1.515154207786300944 ) ) ;
#10313 = CARTESIAN_POINT ( 'NONE',  ( -4.243569643750000786, -25.93287794636623644, -12.75450788076862452 ) ) ;
#10314 = CARTESIAN_POINT ( 'NONE',  ( -1.027846397803541700, 17.49680007765647716, 3.346150245485522312 ) ) ;
#10315 = AXIS2_PLACEMENT_3D ( 'NONE', #9205, #5030, #10408 ) ;
#10316 = DIRECTION ( 'NONE',  ( 3.469446951953612217E-16, -0.000000000000000000, 1.000000000000000000 ) ) ;
#10317 = CIRCLE ( 'NONE', #9682, 0.9999999999999991118 ) ;
#10318 = CARTESIAN_POINT ( 'NONE',  ( -9.000000000000001776, 18.79999999999999361, 2.499999999999998224 ) ) ;
#10319 = EDGE_CURVE ( 'NONE', #15990, #10466, #3177, .T. ) ;
#10320 = EDGE_LOOP ( 'NONE', ( #4657, #7218, #7920, #14990 ) ) ;
#10321 = CARTESIAN_POINT ( 'NONE',  ( 1.135272562821090458, 39.74680007765648071, 3.311245368580554072 ) ) ;
#10322 = CARTESIAN_POINT ( 'NONE',  ( 2.121784821874994176, -29.14763035506834044, -10.93841495796388763 ) ) ;
#10323 = EDGE_CURVE ( 'NONE', #12341, #6360, #18003, .T. ) ;
#10324 = CARTESIAN_POINT ( 'NONE',  ( -4.243569643750000786, -24.64233096457639505, -10.91141578111838584 ) ) ;
#10325 = DIRECTION ( 'NONE',  ( 1.000000000000000000, 0.000000000000000000, 0.000000000000000000 ) ) ;
#10326 = ADVANCED_FACE ( 'NONE', ( #11326 ), #10976, .F. ) ;
#10327 = AXIS2_PLACEMENT_3D ( 'NONE', #9976, #12680, #11103 ) ;
#10328 = FACE_OUTER_BOUND ( 'NONE', #1902, .T. ) ;
#10329 = CARTESIAN_POINT ( 'NONE',  ( -6.158835246850665095E-15, -22.64013793229036864, -15.02577497543054186 ) ) ;
#10330 = CARTESIAN_POINT ( 'NONE',  ( 4.243569643750000786, -23.48083868096554028, -9.252632891433169249 ) ) ;
#10331 = DIRECTION ( 'NONE',  ( 0.000000000000000000, 0.000000000000000000, 1.000000000000000000 ) ) ;
#10332 = CYLINDRICAL_SURFACE ( 'NONE', #9751, 0.9999999999999991118 ) ;
#10333 = CARTESIAN_POINT ( 'NONE',  ( 2.518350579753628971, 24.37180007765648071, 0.7558219633769073242 ) ) ;
#10334 = ORIENTED_EDGE ( 'NONE', *, *, #16935, .F. ) ;
#10335 = CARTESIAN_POINT ( 'NONE',  ( 2.798362969681366330, 21.49680007765647716, -2.102939460078824929 ) ) ;
#10336 = CARTESIAN_POINT ( 'NONE',  ( 1.533898589781675205E-14, -27.25753381391755426, -7.672525335146852754 ) ) ;
#10337 = DIRECTION ( 'NONE',  ( 1.000000000000000000, 0.000000000000000000, 0.000000000000000000 ) ) ;
#10338 = CARTESIAN_POINT ( 'NONE',  ( -5.279047395330986450E-15, -29.57119263748722204, -9.897923940636554008 ) ) ;
#10339 = CIRCLE ( 'NONE', #17173, 3.047499999999999876 ) ;
#10340 = CARTESIAN_POINT ( 'NONE',  ( 8.500000000000001776, 14.80000000000000071, -22.69999999999999929 ) ) ;
#10341 = CARTESIAN_POINT ( 'NONE',  ( 3.518350579753605434, 18.12819992234353705, -1.080741659609877114 ) ) ;
#10342 = ORIENTED_EDGE ( 'NONE', *, *, #4624, .T. ) ;
#10343 = CARTESIAN_POINT ( 'NONE',  ( -2.121784821875005722, -26.35144522785700616, -6.945048742055040414 ) ) ;
#10344 = CIRCLE ( 'NONE', #8279, 1.610000000000000098 ) ;
#10345 = CARTESIAN_POINT ( 'NONE',  ( 3.673772985318219053, 39.49680007765648071, 2.599342558260951730 ) ) ;
#10346 = EDGE_CURVE ( 'NONE', #4066, #1806, #12632, .T. ) ;
#10347 = VERTEX_POINT ( 'NONE', #29 ) ;
#10348 = LINE ( 'NONE', #8866, #4794 ) ;
#10349 = CARTESIAN_POINT ( 'NONE',  ( -4.000000000000004441, -24.36703810445001750, -6.491938924580010983 ) ) ;
#10350 = CARTESIAN_POINT ( 'NONE',  ( -2.121784821874996396, -22.22341586131136992, -13.86408216537410354 ) ) ;
#10351 = CARTESIAN_POINT ( 'NONE',  ( -2.000000000000005773, -28.13060765457947809, -9.853714322293496863 ) ) ;
#10352 = DIRECTION ( 'NONE',  ( 0.000000000000000000, 0.8191520442889952403, -0.5735764363510413855 ) ) ;
#10353 = CYLINDRICAL_SURFACE ( 'NONE', #6723, 8.000000000000000000 ) ;
#10354 = CARTESIAN_POINT ( 'NONE',  ( 4.730628863548789710E-15, -17.88603089060359963, -9.805399520805213598 ) ) ;
#10355 = ORIENTED_EDGE ( 'NONE', *, *, #4911, .F. ) ;
#10356 = DIRECTION ( 'NONE',  ( -0.000000000000000000, 1.000000000000000000, -0.000000000000000000 ) ) ;
#10357 =( NAMED_UNIT ( * ) SI_UNIT ( $, .STERADIAN. ) SOLID_ANGLE_UNIT ( ) );
#10358 = CIRCLE ( 'NONE', #2680, 0.9999999999999991118 ) ;
#10359 = CARTESIAN_POINT ( 'NONE',  ( 0.000000000000000000, 9.254131787996968228, 30.52396275209373044 ) ) ;
#10360 = ORIENTED_EDGE ( 'NONE', *, *, #5974, .F. ) ;
#10361 = ORIENTED_EDGE ( 'NONE', *, *, #6294, .F. ) ;
#10362 = CARTESIAN_POINT ( 'NONE',  ( 0.000000000000000000, 5.977523610840987267, 32.81826849749789687 ) ) ;
#10363 = CARTESIAN_POINT ( 'NONE',  ( -8.500000000000010658, 13.00000000000000178, 20.49999999999998934 ) ) ;
#10364 =( NAMED_UNIT ( * ) PLANE_ANGLE_UNIT ( ) SI_UNIT ( $, .RADIAN. ) );
#10365 = CARTESIAN_POINT ( 'NONE',  ( 2.733110507866328920, 26.12819992234354416, 3.862833514489095510 ) ) ;
#10366 = EDGE_CURVE ( 'NONE', #9005, #12967, #507, .T. ) ;
#10367 = CARTESIAN_POINT ( 'NONE',  ( 2.211161402132839182, 37.87819992234353350, -2.942372952327217739 ) ) ;
#10368 = CARTESIAN_POINT ( 'NONE',  ( 2.518350579753611207, 23.12819992234354416, -0.7558219633769606149 ) ) ;
#10369 = ORIENTED_EDGE ( 'NONE', *, *, #13088, .T. ) ;
#10370 = CARTESIAN_POINT ( 'NONE',  ( -2.829195390882805139, 15.87180007765647716, -3.793023760679206102 ) ) ;
#10371 = CARTESIAN_POINT ( 'NONE',  ( 3.999999999999996447, -24.47458368556090491, -6.645529931877427465 ) ) ;
#10372 = ORIENTED_EDGE ( 'NONE', *, *, #4495, .F. ) ;
#10373 = AXIS2_PLACEMENT_3D ( 'NONE', #7431, #1435, #8451 ) ;
#10374 = CARTESIAN_POINT ( 'NONE',  ( 8.499999999999992895, 14.99364916731036956, 20.49999999999999645 ) ) ;
#10375 = CARTESIAN_POINT ( 'NONE',  ( -3.518350579753630747, 30.62180007765647716, -1.080741659609802729 ) ) ;
#10376 = DIRECTION ( 'NONE',  ( -0.000000000000000000, -0.5735764363510414965, -0.8191520442889950182 ) ) ;
#10377 = CARTESIAN_POINT ( 'NONE',  ( -4.243569643749998122, -20.07580224852517858, -8.661227009200541005 ) ) ;
#10378 = CARTESIAN_POINT ( 'NONE',  ( 0.05938372350929014415, 32.37180007765647360, 4.731580009072201776 ) ) ;
#10379 = CARTESIAN_POINT ( 'NONE',  ( 4.299564228933482956E-15, -16.63909446626264454, -6.455396711050170211 ) ) ;
#10380 = ORIENTED_EDGE ( 'NONE', *, *, #11179, .T. ) ;
#10381 = CARTESIAN_POINT ( 'NONE',  ( -2.864755990943265829, 28.24680007765648071, -2.011557305968488141 ) ) ;
#10382 = CARTESIAN_POINT ( 'NONE',  ( 2.978814741686848677, -10.00000000000000178, 22.09987478887119394 ) ) ;
#10383 = DIRECTION ( 'NONE',  ( 1.000000000000000000, 0.000000000000000000, 0.000000000000000000 ) ) ;
#10384 = PLANE ( 'NONE',  #4205 ) ;
#10385 = FILL_AREA_STYLE_COLOUR ( '', #2326 ) ;
#10386 = ORIENTED_EDGE ( 'NONE', *, *, #17640, .F. ) ;
#10387 = VECTOR ( 'NONE', #17985, 1000.000000000000000 ) ;
#10388 = CARTESIAN_POINT ( 'NONE',  ( -2.864755990943222308, 26.75319992234354771, 2.011557305968548093 ) ) ;
#10389 = CARTESIAN_POINT ( 'NONE',  ( 8.500000000000019540, 0.000000000000000000, 22.49999999999999289 ) ) ;
#10390 = CARTESIAN_POINT ( 'NONE',  ( 4.243569643749996345, -23.44441649529964877, -4.929126507931827383 ) ) ;
#10391 = CARTESIAN_POINT ( 'NONE',  ( 2.055738996568313048, 19.49680007765648071, 1.423772053676023441 ) ) ;
#10392 =( BOUNDED_CURVE ( )  B_SPLINE_CURVE ( 2, ( #8874, #12795, #5569, #8974, #13142, #5662, #9063, #4608, #11219 ),
 .UNSPECIFIED., .F., .T. ) 
 B_SPLINE_CURVE_WITH_KNOTS ( ( 3, 2, 2, 2, 3 ),
 ( 0.2844827586206896686, 0.2873563218390804419, 0.2931034482758620441, 0.2988505747126437018, 0.3017241379310345306 ),
 .UNSPECIFIED. ) 
 CURVE ( )  GEOMETRIC_REPRESENTATION_ITEM ( )  RATIONAL_B_SPLINE_CURVE ( ( 0.9330127018922194093, 0.9330127018922200755, 1.000000000000000000, 0.8660254037844387076, 1.000000000000000000, 0.8660254037844387076, 1.000000000000000000, 0.9330127018922187432, 0.9330127018922194093 ) ) 
 REPRESENTATION_ITEM ( '' )  );
#10393 = EDGE_CURVE ( 'NONE', #12581, #10307, #5500, .T. ) ;
#10394 = CARTESIAN_POINT ( 'NONE',  ( -2.733110507866328476, 17.37819992234354416, -3.862833514489096398 ) ) ;
#10395 = CARTESIAN_POINT ( 'NONE',  ( 4.730628863548789710E-15, -23.04821881776297232, -17.17776791940616832 ) ) ;
#10396 = CARTESIAN_POINT ( 'NONE',  ( 1.999999999999994449, -29.57171845020653222, -11.91183383256282724 ) ) ;
#10397 = EDGE_CURVE ( 'NONE', #11296, #3728, #14032, .T. ) ;
#10398 = CARTESIAN_POINT ( 'NONE',  ( -2.121784821874996396, -18.35177491594184218, -8.334805866423387499 ) ) ;
#10399 = ADVANCED_FACE ( 'NONE', ( #16654 ), #12282, .F. ) ;
#10400 = LINE ( 'NONE', #11600, #15451 ) ;
#10401 = CIRCLE ( 'NONE', #1825, 10.00000000000000000 ) ;
#10402 = ADVANCED_FACE ( 'NONE', ( #15985 ), #10023, .F. ) ;
#10403 = CARTESIAN_POINT ( 'NONE',  ( -1.448116719718852696, -10.00000000000000355, -4.839896329767194416 ) ) ;
#10404 = DIRECTION ( 'NONE',  ( 0.000000000000000000, -0.000000000000000000, -1.000000000000000000 ) ) ;
#10405 = CARTESIAN_POINT ( 'NONE',  ( -9.000000000000003553, 18.79999999999999361, -2.500000000000001776 ) ) ;
#10406 = ORIENTED_EDGE ( 'NONE', *, *, #7671, .F. ) ;
#10407 = EDGE_LOOP ( 'NONE', ( #17548, #1380, #14953, #9785 ) ) ;
#10408 = DIRECTION ( 'NONE',  ( 0.000000000000000000, -0.000000000000000000, 1.000000000000000000 ) ) ;
#10409 = FACE_OUTER_BOUND ( 'NONE', #13034, .T. ) ;
#10410 = DIRECTION ( 'NONE',  ( 0.000000000000000000, -0.000000000000000000, 1.000000000000000000 ) ) ;
#10411 = ORIENTED_EDGE ( 'NONE', *, *, #3454, .F. ) ;
#10412 = CARTESIAN_POINT ( 'NONE',  ( -0.05938372350921170689, 26.37819992234355126, 2.628655560595669183 ) ) ;
#10413 = CARTESIAN_POINT ( 'NONE',  ( -4.243569643750000786, -25.15854975729233090, -11.64865262097848309 ) ) ;
#10414 = CARTESIAN_POINT ( 'NONE',  ( -2.211161402132902243, 23.37180007765647716, -2.942372952327172886 ) ) ;
#10415 = CARTESIAN_POINT ( 'NONE',  ( 9.000000000000001776, 23.19999999999999574, -2.500000000000002665 ) ) ;
#10416 = CARTESIAN_POINT ( 'NONE',  ( 6.660876705454565894, -10.00000000000000178, -8.457461752749473760 ) ) ;
#10417 = CARTESIAN_POINT ( 'NONE',  ( 3.500000000000000444, 39.24680007765647360, -0.05647727720536935281 ) ) ;
#10418 = CARTESIAN_POINT ( 'NONE',  ( 4.243569643750000786, -24.80364933730013277, -11.14180229357466345 ) ) ;
#10419 = CIRCLE ( 'NONE', #17568, 0.9999999999999991118 ) ;
#10420 = DIRECTION ( 'NONE',  ( 0.000000000000000000, 0.000000000000000000, 1.000000000000000000 ) ) ;
#10421 = AXIS2_PLACEMENT_3D ( 'NONE', #16064, #1975, #13357 ) ;
#10422 = CARTESIAN_POINT ( 'NONE',  ( -4.243569643750004339, -26.88587511340589131, -9.844038773665804598 ) ) ;
#10423 = DIRECTION ( 'NONE',  ( 0.000000000000000000, 0.000000000000000000, 1.000000000000000000 ) ) ;
#10424 = PRODUCT_DEFINITION_FORMATION_WITH_SPECIFIED_SOURCE ( 'ANY', '', #6792, .NOT_KNOWN. ) ;
#10425 = DIRECTION ( 'NONE',  ( 0.8191520442889951292, 0.4698463103929522156, -0.3289899283371602867 ) ) ;
#10426 = DIRECTION ( 'NONE',  ( -0.000000000000000000, 0.5000000000000000000, 0.8660254037844385966 ) ) ;
#10427 = CARTESIAN_POINT ( 'NONE',  ( 2.121784821874994176, -26.01805392422797070, -6.468916616312057499 ) ) ;
#10428 = DIRECTION ( 'NONE',  ( -0.000000000000000000, -1.000000000000000000, -0.000000000000000000 ) ) ;
#10429 = CARTESIAN_POINT ( 'NONE',  ( 0.8262555684461332373, 27.24680007765648426, 2.360188852285403982 ) ) ;
#10430 = LINE ( 'NONE', #9675, #12671 ) ;
#10431 = CARTESIAN_POINT ( 'NONE',  ( 2.798362969681366330, 31.49680007765647716, -2.102939460078824929 ) ) ;
#10432 = ADVANCED_FACE ( 'NONE', ( #3372 ), #7003, .T. ) ;
#10433 = CARTESIAN_POINT ( 'NONE',  ( 8.500000000000001776, 15.00000000000000178, -20.49999999999999645 ) ) ;
#10434 = CIRCLE ( 'NONE', #15485, 0.4000000000000001887 ) ;
#10435 = SURFACE_STYLE_USAGE ( .BOTH. , #17233 ) ;
#10436 = CARTESIAN_POINT ( 'NONE',  ( -4.000000000000000888, -25.33599996764090534, -11.90207778518377246 ) ) ;
#10437 = CIRCLE ( 'NONE', #11316, 3.000000000000000444 ) ;
#10438 = DIRECTION ( 'NONE',  ( 0.000000000000000000, 0.000000000000000000, -1.000000000000000000 ) ) ;
#10439 = CARTESIAN_POINT ( 'NONE',  ( -2.211161402132839182, 19.12819992234353705, 2.942372952327218627 ) ) ;
#10440 = EDGE_LOOP ( 'NONE', ( #4012, #15729, #10270, #3774 ) ) ;
#10441 = CARTESIAN_POINT ( 'NONE',  ( -4.243569643749998122, -20.88239411214383523, -9.813159571481939736 ) ) ;
#10442 = CARTESIAN_POINT ( 'NONE',  ( -2.864755990943265829, 15.74680007765647716, -2.011557305968488141 ) ) ;
#10443 = EDGE_LOOP ( 'NONE', ( #16379, #6422 ) ) ;
#10444 = DIRECTION ( 'NONE',  ( -1.000000000000000000, 0.000000000000000000, -0.000000000000000000 ) ) ;
#10445 = CARTESIAN_POINT ( 'NONE',  ( -8.000000000000003553, 40.79999999999999716, -2.500000000000001776 ) ) ;
#10446 = CARTESIAN_POINT ( 'NONE',  ( -4.243569643750000786, -25.19081343183707844, -11.69472992346973861 ) ) ;
#10447 = CARTESIAN_POINT ( 'NONE',  ( -6.938893903907228378E-15, 6.938893903907228378E-15, 30.00000000000000000 ) ) ;
#10448 = CIRCLE ( 'NONE', #5413, 6.000000000000000888 ) ;
#10449 = LINE ( 'NONE', #9059, #1179 ) ;
#10450 = CARTESIAN_POINT ( 'NONE',  ( -1.661723472263481630E-14, -20.31715336506863423, -11.70820919606011579 ) ) ;
#10451 = CARTESIAN_POINT ( 'NONE',  ( -5.330712181944245322E-15, -30.91467592037801282, -11.32627250406271635 ) ) ;
#10452 = EDGE_CURVE ( 'NONE', #2269, #2204, #7902, .T. ) ;
#10453 = ORIENTED_EDGE ( 'NONE', *, *, #9197, .T. ) ;
#10454 = CARTESIAN_POINT ( 'NONE',  ( -8.500000000000005329, 10.00000000000000000, -20.49999999999999645 ) ) ;
#10455 = CARTESIAN_POINT ( 'NONE',  ( -4.000000000000004441, -24.88325689716596045, -7.229175764440105567 ) ) ;
#10456 = CARTESIAN_POINT ( 'NONE',  ( -5.577813053751546416E-15, -25.38624068961733826, -5.000041789647243107 ) ) ;
#10457 = EDGE_CURVE ( 'NONE', #16267, #15166, #809, .T. ) ;
#10458 = VERTEX_POINT ( 'NONE', #14502 ) ;
#10459 = EDGE_LOOP ( 'NONE', ( #5153, #8021 ) ) ;
#10460 = CARTESIAN_POINT ( 'NONE',  ( 0.000000000000000000, 5.977523610840987267, 32.81826849749789687 ) ) ;
#10461 = EDGE_CURVE ( 'NONE', #8594, #2439, #4646, .T. ) ;
#10462 = CARTESIAN_POINT ( 'NONE',  ( 1.444289557195957086, 25.25319992234354771, -4.262301884875733471 ) ) ;
#10463 = CARTESIAN_POINT ( 'NONE',  ( 3.518350579753606322, 38.12819992234353350, -1.080741659609876892 ) ) ;
#10464 = CARTESIAN_POINT ( 'NONE',  ( -1.497042530366522461, 19.87819992234354771, -2.161531897785030409 ) ) ;
#10465 = AXIS2_PLACEMENT_3D ( 'NONE', #717, #13490, #12099 ) ;
#10466 = VERTEX_POINT ( 'NONE', #7430 ) ;
#10467 = CARTESIAN_POINT ( 'NONE',  ( 3.673772985318219053, 16.99680007765647716, 2.599342558260951730 ) ) ;
#10468 = CARTESIAN_POINT ( 'NONE',  ( 4.000000000000000888, -22.56132395608780783, -7.939429769928989522 ) ) ;
#10469 = ORIENTED_EDGE ( 'NONE', *, *, #9374, .T. ) ;
#10470 = CARTESIAN_POINT ( 'NONE',  ( 0.000000000000000000, 0.7216878364870329410, -1.250000000000000000 ) ) ;
#10471 = DIRECTION ( 'NONE',  ( 0.000000000000000000, 0.000000000000000000, 1.000000000000000000 ) ) ;
#10472 = CARTESIAN_POINT ( 'NONE',  ( 9.184850993605147944E-16, -10.54254386713301628, 22.30101802474215589 ) ) ;
#10473 = CARTESIAN_POINT ( 'NONE',  ( 4.243569643750003451, -18.87129173218799849, -6.941007716193646537 ) ) ;
#10474 = CARTESIAN_POINT ( 'NONE',  ( 4.730628863548789710E-15, -19.95090606146734658, -12.75434688024559726 ) ) ;
#10475 = AXIS2_PLACEMENT_3D ( 'NONE', #8091, #1063, #13842 ) ;
#10476 = PRODUCT_DEFINITION_SHAPE ( 'NONE', 'NONE',  #16042 ) ;
#10477 = CARTESIAN_POINT ( 'NONE',  ( 1.071796769724487675, -29.82710107677840483, -11.34224769979141456 ) ) ;
#10478 = ORIENTED_EDGE ( 'NONE', *, *, #17463, .T. ) ;
#10479 = CARTESIAN_POINT ( 'NONE',  ( 1.533898589781675205E-14, -28.48355344591296401, -9.423462828807814162 ) ) ;
#10480 =( NAMED_UNIT ( * ) SI_UNIT ( $, .STERADIAN. ) SOLID_ANGLE_UNIT ( ) );
#10481 = CARTESIAN_POINT ( 'NONE',  ( -9.000000000000001776, 16.59999999999999787, 2.499999999999995559 ) ) ;
#10482 = CARTESIAN_POINT ( 'NONE',  ( 1.071796769724494780, -28.21391734883615143, -9.038382574221850874 ) ) ;
#10483 = EDGE_LOOP ( 'NONE', ( #6025, #15061 ) ) ;
#10484 = CARTESIAN_POINT ( 'NONE',  ( 2.798362969681409851, 23.50319992234354416, 2.102939460078764977 ) ) ;
#10485 = DIRECTION ( 'NONE',  ( 0.000000000000000000, -1.000000000000000000, 0.000000000000000000 ) ) ;
#10486 = CARTESIAN_POINT ( 'NONE',  ( -4.243569643749997233, -19.55958345580923918, -7.923990169340445533 ) ) ;
#10487 = CARTESIAN_POINT ( 'NONE',  ( 2.518350579753628971, 21.87180007765647360, 0.7558219633769073242 ) ) ;
#10488 = EDGE_CURVE ( 'NONE', #1681, #8512, #15602, .T. ) ;
#10489 = CARTESIAN_POINT ( 'NONE',  ( -2.211161402132839182, 39.12819992234354771, 2.942372952327218627 ) ) ;
#10490 = CARTESIAN_POINT ( 'NONE',  ( 2.121784821875004390, -23.29887167946958115, -15.39999224841596437 ) ) ;
#10491 = CARTESIAN_POINT ( 'NONE',  ( 2.000000000000004441, -24.06853954178204447, -16.13143356498672887 ) ) ;
#10492 = CARTESIAN_POINT ( 'NONE',  ( 2.121784821874994176, -24.24355182426693389, -3.934664979292979314 ) ) ;
#10493 = DIRECTION ( 'NONE',  ( -0.000000000000000000, -1.000000000000000000, -0.000000000000000000 ) ) ;
#10494 = DIRECTION ( 'NONE',  ( -3.469446951953613696E-16, -0.000000000000000000, -1.000000000000000000 ) ) ;
#10495 = FACE_OUTER_BOUND ( 'NONE', #13400, .T. ) ;
#10496 = DIRECTION ( 'NONE',  ( -0.000000000000000000, -1.000000000000000000, -0.000000000000000000 ) ) ;
#10497 = VERTEX_POINT ( 'NONE', #10303 ) ;
#10498 = ORIENTED_EDGE ( 'NONE', *, *, #238, .F. ) ;
#10499 =( BOUNDED_CURVE ( )  B_SPLINE_CURVE ( 3, ( #3047, #1844, #3133, #6089 ),
 .UNSPECIFIED., .F., .F. ) 
 B_SPLINE_CURVE_WITH_KNOTS ( ( 4, 4 ),
 ( 2.111895852752041502, 3.141592653589793116 ),
 .UNSPECIFIED. ) 
 CURVE ( )  GEOMETRIC_REPRESENTATION_ITEM ( )  RATIONAL_B_SPLINE_CURVE ( ( 1.000000000000000000, 0.9135782535825734962, 0.9135782535825734962, 1.000000000000000000 ) ) 
 REPRESENTATION_ITEM ( '' )  );
#10500 = CARTESIAN_POINT ( 'NONE',  ( 4.243569643749996345, -21.89576011715183768, -2.717415988351541856 ) ) ;
#10501 = EDGE_CURVE ( 'NONE', #15166, #3191, #15320, .T. ) ;
#10502 = CYLINDRICAL_SURFACE ( 'NONE', #5622, 4.000000000000000000 ) ;
#10503 = CARTESIAN_POINT ( 'NONE',  ( 1.071796769724495224, -17.23136730949185491, -7.301249991555458507 ) ) ;
#10504 = ORIENTED_EDGE ( 'NONE', *, *, #1293, .F. ) ;
#10505 = CARTESIAN_POINT ( 'NONE',  ( 2.055738996568281518, 30.50319992234354771, -1.423772053676066518 ) ) ;
#10506 = SHAPE_REPRESENTATION_RELATIONSHIP ( 'NONE' , 'NONE' ,  #17791, #6498 ) ;
#10507 = CARTESIAN_POINT ( 'NONE',  ( -2.121784821874996396, -22.70737097948255823, -14.55524170274294171 ) ) ;
#10508 = CARTESIAN_POINT ( 'NONE',  ( 1.027846397803542144, 26.24680007765648071, -3.346150245485522312 ) ) ;
#10509 = EDGE_CURVE ( 'NONE', #10807, #10740, #10586, .T. ) ;
#10510 = DIRECTION ( 'NONE',  ( 0.000000000000000000, -1.224646799147353207E-16, 1.000000000000000000 ) ) ;
#10511 = CARTESIAN_POINT ( 'NONE',  ( -4.000000000000000888, -23.98092563605662875, -9.966831079544254735 ) ) ;
#10512 = CARTESIAN_POINT ( 'NONE',  ( 4.243569643749996345, -27.09021171885596146, -10.13586168944375210 ) ) ;
#10513 = DIRECTION ( 'NONE',  ( -0.000000000000000000, -1.000000000000000000, -0.000000000000000000 ) ) ;
#10514 = CARTESIAN_POINT ( 'NONE',  ( 4.730628863548789710E-15, -20.69297057599650458, -13.81412483754448495 ) ) ;
#10515 = DIRECTION ( 'NONE',  ( 0.000000000000000000, -0.000000000000000000, -1.000000000000000000 ) ) ;
#10516 = DIRECTION ( 'NONE',  ( -0.000000000000000000, -1.000000000000000000, -0.000000000000000000 ) ) ;
#10517 = CARTESIAN_POINT ( 'NONE',  ( 2.000000000000004441, -23.10062930614460797, -14.74911449125581520 ) ) ;
#10518 = CARTESIAN_POINT ( 'NONE',  ( 4.730628863548789710E-15, -19.91864238692259903, -12.70826957775434352 ) ) ;
#10519 = AXIS2_PLACEMENT_3D ( 'NONE', #17098, #1602, #3084 ) ;
#10520 = CARTESIAN_POINT ( 'NONE',  ( -31.74999999999995737, 4.898587196589415787E-16, -4.000000000000001776 ) ) ;
#10521 = CARTESIAN_POINT ( 'NONE',  ( -1.734723475976807094E-15, 31.99999999999999289, -2.500000000000000000 ) ) ;
#10522 = CARTESIAN_POINT ( 'NONE',  ( 1.497042530366477164, 31.37180007765648426, -2.161531897785062384 ) ) ;
#10523 = EDGE_CURVE ( 'NONE', #16355, #17896, #3419, .T. ) ;
#10524 = ORIENTED_EDGE ( 'NONE', *, *, #4650, .F. ) ;
#10525 = CARTESIAN_POINT ( 'NONE',  ( -2.115076519116362519, 27.62180007765648071, 3.012182706137108035 ) ) ;
#10526 = CARTESIAN_POINT ( 'NONE',  ( 0.000000000000000000, 5.977523610840987267, 32.81826849749789687 ) ) ;
#10527 = CONTEXT_DEPENDENT_SHAPE_REPRESENTATION ( #15540, #17915 ) ;
#10528 = CARTESIAN_POINT ( 'NONE',  ( 1.027846397803612311, 21.25319992234354416, 3.346150245485499219 ) ) ;
#10529 = ORIENTED_EDGE ( 'NONE', *, *, #14377, .F. ) ;
#10530 = CARTESIAN_POINT ( 'NONE',  ( 4.730628863548789710E-15, -18.40224968331953548, -10.54263636066531085 ) ) ;
#10531 = CARTESIAN_POINT ( 'NONE',  ( -2.798362969681365886, 17.74680007765647716, 2.102939460078824929 ) ) ;
#10532 = ORIENTED_EDGE ( 'NONE', *, *, #2769, .T. ) ;
#10533 = AXIS2_PLACEMENT_3D ( 'NONE', #11341, #9651, #6783 ) ;
#10534 = DIRECTION ( 'NONE',  ( -0.000000000000000000, 1.000000000000000000, -0.000000000000000000 ) ) ;
#10535 = DIRECTION ( 'NONE',  ( 0.000000000000000000, 0.000000000000000000, 1.000000000000000000 ) ) ;
#10536 = CARTESIAN_POINT ( 'NONE',  ( 4.243569643750003451, -24.06574333389212228, -14.35945341728585767 ) ) ;
#10537 = CARTESIAN_POINT ( 'NONE',  ( 5.348585110054253633, -10.20669165899109743, -1.142694657456339691 ) ) ;
#10538 = DIRECTION ( 'NONE',  ( -0.000000000000000000, -1.000000000000000000, -0.000000000000000000 ) ) ;
#10539 = CARTESIAN_POINT ( 'NONE',  ( 4.243569643750003451, -18.12922721765884049, -5.881229758894760629 ) ) ;
#10540 = EDGE_LOOP ( 'NONE', ( #17062, #5202, #13491, #18303 ) ) ;
#10541 = CARTESIAN_POINT ( 'NONE',  ( 1.071796769724504328, -26.47167892412480583, -6.550208240700799323 ) ) ;
#10542 = CARTESIAN_POINT ( 'NONE',  ( -4.000000000000004441, -24.62514750080799075, -6.860557344510057831 ) ) ;
#10543 = ORIENTED_EDGE ( 'NONE', *, *, #17831, .T. ) ;
#10544 = ORIENTED_EDGE ( 'NONE', *, *, #2661, .F. ) ;
#10545 = CARTESIAN_POINT ( 'NONE',  ( -1.071796769724505882, -18.17622414369163053, -8.650645395974535745 ) ) ;
#10546 = DIRECTION ( 'NONE',  ( 0.000000000000000000, 0.000000000000000000, 1.000000000000000000 ) ) ;
#10547 = FILL_AREA_STYLE_COLOUR ( '', #2444 ) ;
#10548 = CARTESIAN_POINT ( 'NONE',  ( 2.829195390882724759, 22.87819992234354416, -3.793023760679264278 ) ) ;
#10549 = CARTESIAN_POINT ( 'NONE',  ( 2.798362969681409851, 33.50319992234354771, 2.102939460078764977 ) ) ;
#10550 = VECTOR ( 'NONE', #9868, 1000.000000000000000 ) ;
#10551 = CARTESIAN_POINT ( 'NONE',  ( -2.518350579753611207, 21.87819992234354416, 0.7558219633769609480 ) ) ;
#10552 = ORIENTED_EDGE ( 'NONE', *, *, #8542, .F. ) ;
#10553 = CARTESIAN_POINT ( 'NONE',  ( 3.607379964056306676, 18.99680007765647716, -2.690724712371305838 ) ) ;
#10554 = CARTESIAN_POINT ( 'NONE',  ( -4.000000000000000888, -22.69037865426678380, -8.123738979894017831 ) ) ;
#10555 = ORIENTED_EDGE ( 'NONE', *, *, #8455, .T. ) ;
#10556 = EDGE_CURVE ( 'NONE', #5725, #5839, #5534, .T. ) ;
#10557 = DIRECTION ( 'NONE',  ( -0.000000000000000000, -1.000000000000000000, -0.000000000000000000 ) ) ;
#10558 = EDGE_CURVE ( 'NONE', #6382, #10757, #13277, .T. ) ;
#10559 = CARTESIAN_POINT ( 'NONE',  ( 1.135272562821090458, 37.24680007765648071, 3.311245368580554072 ) ) ;
#10560 = CARTESIAN_POINT ( 'NONE',  ( 0.000000000000000000, 48.00000000000000000, -16.00000000000000000 ) ) ;
#10561 = EDGE_CURVE ( 'NONE', #297, #11364, #15908, .T. ) ;
#10562 = CARTESIAN_POINT ( 'NONE',  ( 4.243569643750000786, -20.38352592466991808, -4.829211852272596417 ) ) ;
#10563 = VECTOR ( 'NONE', #14784, 1000.000000000000000 ) ;
#10564 = CARTESIAN_POINT ( 'NONE',  ( -2.121784821875005722, -27.38388281328888141, -8.419522421775232246 ) ) ;
#10565 = EDGE_CURVE ( 'NONE', #16355, #16719, #6234, .T. ) ;
#10566 = CARTESIAN_POINT ( 'NONE',  ( 0.4488142760818575883, -30.27607861724349902, -12.00111911307740087 ) ) ;
#10567 = VERTEX_POINT ( 'NONE', #11883 ) ;
#10568 = CARTESIAN_POINT ( 'NONE',  ( 5.694236848974395748, -11.38679575279332212, 16.60313092159397641 ) ) ;
#10569 = CARTESIAN_POINT ( 'NONE',  ( -10.00000000000000178, 23.19999999999999574, -2.500000000000001776 ) ) ;
#10570 = CARTESIAN_POINT ( 'NONE',  ( 0.000000000000000000, 13.00000000000000178, 2.500000000000000000 ) ) ;
#10571 = CARTESIAN_POINT ( 'NONE',  ( -2.121784821875005722, -29.96497677686856775, -12.10570662107570961 ) ) ;
#10572 = ORIENTED_EDGE ( 'NONE', *, *, #2155, .F. ) ;
#10573 = CARTESIAN_POINT ( 'NONE',  ( 2.798362969681409851, 31.00319992234354416, 2.102939460078764977 ) ) ;
#10574 = DIRECTION ( 'NONE',  ( -0.000000000000000000, -1.000000000000000000, -0.000000000000000000 ) ) ;
#10575 = CARTESIAN_POINT ( 'NONE',  ( -4.243569643750005227, -23.53045296075229942, -5.051999314575184030 ) ) ;
#10576 = CARTESIAN_POINT ( 'NONE',  ( -2.500000000000001332, 25.49680007765647716, 0.05647727720535858364 ) ) ;
#10577 = EDGE_CURVE ( 'NONE', #3191, #9017, #14691, .T. ) ;
#10578 = CARTESIAN_POINT ( 'NONE',  ( -4.481649420246396787, 14.62819992234354594, -1.518615910253363399 ) ) ;
#10579 = CARTESIAN_POINT ( 'NONE',  ( -2.121784821875005722, -29.44875798415262835, -11.36846978121561236 ) ) ;
#10580 = AXIS2_PLACEMENT_3D ( 'NONE', #17247, #15324, #2624 ) ;
#10581 = CARTESIAN_POINT ( 'NONE',  ( -2.000000000000005773, -29.61473668293285399, -11.97327023588450601 ) ) ;
#10582 = PRODUCT_RELATED_PRODUCT_CATEGORY ( 'part', '', ( #2369 ) ) ;
#10583 = CARTESIAN_POINT ( 'NONE',  ( -2.121784821875005722, -24.28657005699325921, -3.996101382614658970 ) ) ;
#10584 = CARTESIAN_POINT ( 'NONE',  ( -3.500000000000000444, 15.49680007765647893, 0.05647727720536892260 ) ) ;
#10585 = CLOSED_SHELL ( 'NONE', ( #12149, #2330, #12874, #2820, #382, #12914, #17574, #11917, #4164, #8187 ) ) ;
#10586 = LINE ( 'NONE', #9196, #13526 ) ;
#10587 = CARTESIAN_POINT ( 'NONE',  ( 1.743066579297358403E-15, -23.60804816792780159, -16.40809404916146264 ) ) ;
#10588 = MECHANICAL_DESIGN_GEOMETRIC_PRESENTATION_REPRESENTATION (  '', ( #2021 ), #4363 ) ;
#10589 = LINE ( 'NONE', #14879, #1733 ) ;
#10590 = ORIENTED_EDGE ( 'NONE', *, *, #3887, .T. ) ;
#10591 = CIRCLE ( 'NONE', #543, 7.000000000000000000 ) ;
#10592 = ORIENTED_EDGE ( 'NONE', *, *, #16127, .T. ) ;
#10593 = CARTESIAN_POINT ( 'NONE',  ( 4.299564228933482956E-15, -16.44551241969911359, -6.178932897109397970 ) ) ;
#10594 = DIRECTION ( 'NONE',  ( 1.000000000000000000, 0.000000000000000000, -4.336808689942021680E-16 ) ) ;
#10595 = DIRECTION ( 'NONE',  ( -0.000000000000000000, -1.000000000000000000, -0.000000000000000000 ) ) ;
#10596 = ORIENTED_EDGE ( 'NONE', *, *, #8742, .F. ) ;
#10597 = CARTESIAN_POINT ( 'NONE',  ( -1.989345975306457071, 32.25319992234354061, -1.515154207786300944 ) ) ;
#10598 = SURFACE_SIDE_STYLE ('',( #4942 ) ) ;
#10599 = CARTESIAN_POINT ( 'NONE',  ( 4.730628863548789710E-15, -20.95107997235447073, -14.18274325747453268 ) ) ;
#10600 = CARTESIAN_POINT ( 'NONE',  ( -2.798362969681365886, 25.24680007765647716, 2.102939460078824929 ) ) ;
#10601 = CARTESIAN_POINT ( 'NONE',  ( 0.000000000000000000, 3.000000000000000000, 4.000000000000001776 ) ) ;
#10602 = CARTESIAN_POINT ( 'NONE',  ( 1.533898589781675205E-14, -27.19300646412311551, -7.580370729157575482 ) ) ;
#10603 = AXIS2_PLACEMENT_3D ( 'NONE', #6963, #11228, #4280 ) ;
#10604 = CARTESIAN_POINT ( 'NONE',  ( -5.330712181944245322E-15, -29.14017382041697601, -8.792020867043637722 ) ) ;
#10605 = AXIS2_PLACEMENT_3D ( 'NONE', #16749, #1256, #6890 ) ;
#10606 =( BOUNDED_CURVE ( )  B_SPLINE_CURVE ( 2, ( #9414, #10811, #2394, #8025, #13776, #13682, #9602, #12287, #5248 ),
 .UNSPECIFIED., .F., .T. ) 
 B_SPLINE_CURVE_WITH_KNOTS ( ( 3, 2, 2, 2, 3 ),
 ( 0.7155172413793103869, 0.7183908045977011048, 0.7241379310344827624, 0.7298850574712644201, 0.7327586206896552490 ),
 .UNSPECIFIED. ) 
 CURVE ( )  GEOMETRIC_REPRESENTATION_ITEM ( )  RATIONAL_B_SPLINE_CURVE ( ( 0.9330127018922194093, 0.9330127018922206306, 1.000000000000000000, 0.8660254037844387076, 1.000000000000000000, 0.8660254037844387076, 1.000000000000000000, 0.9330127018922180770, 0.9330127018922194093 ) ) 
 REPRESENTATION_ITEM ( '' )  );
#10607 = CARTESIAN_POINT ( 'NONE',  ( 1.300000000000000044, 0.7216878364870329410, 1.249999999999999778 ) ) ;
#10608 = DIRECTION ( 'NONE',  ( 0.000000000000000000, -1.000000000000000000, 9.859324684083080328E-16 ) ) ;
#10609 = LINE ( 'NONE', #6626, #16838 ) ;
#10610 = CARTESIAN_POINT ( 'NONE',  ( 2.121784821874994176, -26.79238211330187625, -7.574771876102201595 ) ) ;
#10611 = ORIENTED_EDGE ( 'NONE', *, *, #1576, .F. ) ;
#10612 = DIRECTION ( 'NONE',  ( 0.000000000000000000, 1.224646799147353207E-16, -1.000000000000000000 ) ) ;
#10613 = LINE ( 'NONE', #17788, #2649 ) ;
#10614 = CIRCLE ( 'NONE', #15370, 8.000000000000001776 ) ;
#10615 = CARTESIAN_POINT ( 'NONE',  ( -0.7188294034286043521, 29.99680007765648071, 2.395093729190366005 ) ) ;
#10616 = AXIS2_PLACEMENT_3D ( 'NONE', #4356, #14573, #11674 ) ;
#10617 = EDGE_LOOP ( 'NONE', ( #7204, #17790, #12589, #9809, #10469 ) ) ;
#10618 = CARTESIAN_POINT ( 'NONE',  ( 0.05938372350927906967, 32.37180007765648071, 3.680117784833935701 ) ) ;
#10619 = DIRECTION ( 'NONE',  ( 1.000000000000000000, 0.000000000000000000, -4.336808689942021680E-16 ) ) ;
#10620 = SHAPE_DEFINITION_REPRESENTATION ( #17461, #7684 ) ;
#10621 = LINE ( 'NONE', #7834, #12524 ) ;
#10622 = ORIENTED_EDGE ( 'NONE', *, *, #2209, .F. ) ;
#10623 = CARTESIAN_POINT ( 'NONE',  ( -2.121784821875005722, -25.83522643514106676, -6.207811902194944054 ) ) ;
#10624 = ADVANCED_FACE ( 'NONE', ( #17579 ), #685, .T. ) ;
#10625 = CARTESIAN_POINT ( 'NONE',  ( 3.500000000000000444, 19.24680007765648071, -0.05647727720536935281 ) ) ;
#10626 = VERTEX_POINT ( 'NONE', #5025 ) ;
#10627 = PRODUCT_DEFINITION_SHAPE ( 'NONE', 'NONE',  #13870 ) ;
#10628 = EDGE_CURVE ( 'NONE', #11984, #2690, #6600, .T. ) ;
#10629 = DIRECTION ( 'NONE',  ( -0.000000000000000000, -1.000000000000000000, -0.000000000000000000 ) ) ;
#10630 = CARTESIAN_POINT ( 'NONE',  ( -3.852824484123190008, -26.05880171954380842, -15.10261301480446683 ) ) ;
#10631 = DIRECTION ( 'NONE',  ( 0.000000000000000000, 0.000000000000000000, 1.000000000000000000 ) ) ;
#10632 = CARTESIAN_POINT ( 'NONE',  ( 7.634387662550983222, -10.16876176238401186, 11.61152380675876650 ) ) ;
#10633 = EDGE_CURVE ( 'NONE', #4165, #14197, #7295, .T. ) ;
#10634 = CARTESIAN_POINT ( 'NONE',  ( -2.121784821875005722, -22.73791367884544812, -1.784390863034371666 ) ) ;
#10635 = ORIENTED_EDGE ( 'NONE', *, *, #10346, .F. ) ;
#10636 = CARTESIAN_POINT ( 'NONE',  ( 9.000000000000000000, 27.59999999999999432, -2.500000000000001332 ) ) ;
#10637 = AXIS2_PLACEMENT_3D ( 'NONE', #232, #7261, #5788 ) ;
#10638 = CARTESIAN_POINT ( 'NONE',  ( -4.000000000000000888, -22.75490600406122255, -8.215893585883295103 ) ) ;
#10639 = ORIENTED_EDGE ( 'NONE', *, *, #11807, .T. ) ;
#10640 = ORIENTED_EDGE ( 'NONE', *, *, #11579, .F. ) ;
#10641 = DIRECTION ( 'NONE',  ( -0.000000000000000000, -1.000000000000000000, -0.000000000000000000 ) ) ;
#10642 = SURFACE_STYLE_FILL_AREA ( #4988 ) ;
#10643 = SHAPE_REPRESENTATION_RELATIONSHIP ( 'NONE' , 'NONE' ,  #4006, #3417 ) ;
#10644 = VECTOR ( 'NONE', #2953, 1000.000000000000000 ) ;
#10645 = CARTESIAN_POINT ( 'NONE',  ( -0.05938372350918959958, 31.37819992234354061, 4.731580009072201776 ) ) ;
#10646 = CARTESIAN_POINT ( 'NONE',  ( 1.135272562821020070, 32.75319992234354771, -3.311245368580577164 ) ) ;
#10647 = AXIS2_PLACEMENT_3D ( 'NONE', #1382, #17056, #14163 ) ;
#10648 = CARTESIAN_POINT ( 'NONE',  ( 0.7188294034286553114, 21.25319992234354771, 2.395093729190349130 ) ) ;
#10649 = VERTEX_POINT ( 'NONE', #7805 ) ;
#10650 = CARTESIAN_POINT ( 'NONE',  ( 4.481649420246366589, 16.62180007765647716, -1.518615910253458212 ) ) ;
#10651 = CARTESIAN_POINT ( 'NONE',  ( -1.999999999999996225, -18.86333338189633579, -8.697628763064102486 ) ) ;
#10652 = EDGE_CURVE ( 'NONE', #1285, #12849, #9670, .T. ) ;
#10653 = ORIENTED_EDGE ( 'NONE', *, *, #17386, .T. ) ;
#10654 = CARTESIAN_POINT ( 'NONE',  ( 9.000000000000000000, 40.79999999999999716, -2.500000000000001332 ) ) ;
#10655 = CARTESIAN_POINT ( 'NONE',  ( -3.500000000000000444, 40.49680007765648071, 0.05647727720536892260 ) ) ;
#10656 = FACE_OUTER_BOUND ( 'NONE', #6555, .T. ) ;
#10657 = AXIS2_PLACEMENT_3D ( 'NONE', #16376, #7823, #10425 ) ;
#10658 = CARTESIAN_POINT ( 'NONE',  ( -2.121784821875005722, -22.70565000430070057, -1.738313560543115477 ) ) ;
#10659 = CARTESIAN_POINT ( 'NONE',  ( 2.121784821874994176, -27.59897397692052934, -8.726704438383601214 ) ) ;
#10660 = DIRECTION ( 'NONE',  ( -0.000000000000000000, -0.5735764363510414965, -0.8191520442889950182 ) ) ;
#10661 = ORIENTED_EDGE ( 'NONE', *, *, #18330, .F. ) ;
#10662 = CARTESIAN_POINT ( 'NONE',  ( 0.7594769011888096166, -10.00000000000000178, 23.07585096715833473 ) ) ;
#10663 = ADVANCED_FACE ( 'NONE', ( #12247 ), #2080, .F. ) ;
#10664 = FACE_OUTER_BOUND ( 'NONE', #8244, .T. ) ;
#10665 = CARTESIAN_POINT ( 'NONE',  ( -2.121784821874996396, -24.03018163581715072, -16.44441110488443769 ) ) ;
#10666 = ORIENTED_EDGE ( 'NONE', *, *, #6834, .F. ) ;
#10667 = CARTESIAN_POINT ( 'NONE',  ( -3.481649420246394122, 27.12819992234354771, -1.193696214020467883 ) ) ;
#10668 = CARTESIAN_POINT ( 'NONE',  ( -8.999999999999996447, -13.00000000000000178, 15.14468620625656925 ) ) ;
#10669 = CARTESIAN_POINT ( 'NONE',  ( -2.121784821875005722, -22.70565000430070057, -1.738313560543115477 ) ) ;
#10670 = CARTESIAN_POINT ( 'NONE',  ( 2.518350579753628971, 24.37180007765648071, 0.7558219633769073242 ) ) ;
#10671 = CIRCLE ( 'NONE', #1507, 4.000000000000001776 ) ;
#10672 = CARTESIAN_POINT ( 'NONE',  ( 4.481649420246397675, 20.87819992234354416, 1.518615910253363177 ) ) ;
#10673 = CARTESIAN_POINT ( 'NONE',  ( 4.000000000000000888, -25.91674610874139972, -12.73146922901961098 ) ) ;
#10674 = EDGE_LOOP ( 'NONE', ( #2415, #7982, #2119, #14945 ) ) ;
#10675 = CARTESIAN_POINT ( 'NONE',  ( -2.121784821875005722, -23.77035126427731981, -3.258864542754563942 ) ) ;
#10676 = CARTESIAN_POINT ( 'NONE',  ( -3.607379964056306676, 35.24680007765647360, 2.690724712371306282 ) ) ;
#10677 = CARTESIAN_POINT ( 'NONE',  ( -8.500000000000007105, 14.80000000000000071, -18.29999999999999716 ) ) ;
#10678 = VECTOR ( 'NONE', #9334, 1000.000000000000000 ) ;
#10679 = CARTESIAN_POINT ( 'NONE',  ( -3.706921591972381904E-14, -16.89720386262061425, -6.824015130980216171 ) ) ;
#10680 = DIRECTION ( 'NONE',  ( 0.000000000000000000, 0.8191520442889952403, -0.5735764363510413855 ) ) ;
#10681 = ORIENTED_EDGE ( 'NONE', *, *, #2280, .T. ) ;
#10682 = ORIENTED_EDGE ( 'NONE', *, *, #13846, .F. ) ;
#10683 = CYLINDRICAL_SURFACE ( 'NONE', #18047, 0.9999999999999991118 ) ;
#10684 = EDGE_CURVE ( 'NONE', #6854, #1143, #6429, .T. ) ;
#10685 = ADVANCED_FACE ( 'NONE', ( #3725 ), #12156, .T. ) ;
#10686 = DIRECTION ( 'NONE',  ( 0.000000000000000000, 0.000000000000000000, -1.000000000000000000 ) ) ;
#10687 = DIRECTION ( 'NONE',  ( 0.000000000000000000, -1.000000000000000000, 0.000000000000000000 ) ) ;
#10688 = ORIENTED_EDGE ( 'NONE', *, *, #8787, .F. ) ;
#10689 = CARTESIAN_POINT ( 'NONE',  ( -2.055738996568281518, 31.75319992234354771, 1.423772053676066962 ) ) ;
#10690 = PRESENTATION_STYLE_ASSIGNMENT (( #7901 ) ) ;
#10691 = EDGE_CURVE ( 'NONE', #17988, #7315, #3528, .T. ) ;
#10692 = CARTESIAN_POINT ( 'NONE',  ( -2.121784821875005722, -29.15838491324991466, -10.95377405879430910 ) ) ;
#10693 = CARTESIAN_POINT ( 'NONE',  ( 2.798362969681366330, 26.49680007765648071, -2.102939460078824929 ) ) ;
#10694 = DIRECTION ( 'NONE',  ( -0.000000000000000000, 1.000000000000000000, -0.000000000000000000 ) ) ;
#10695 = CARTESIAN_POINT ( 'NONE',  ( 2.121784821874994176, -27.85708337327849549, -9.095322858313648950 ) ) ;
#10696 = COLOUR_RGB ( '',0.8941176470588234615, 0.8941176470588234615, 0.8941176470588234615 ) ;
#10697 = CARTESIAN_POINT ( 'NONE',  ( 2.121784821874994176, -28.11519276963646519, -9.463941278243694910 ) ) ;
#10698 = CARTESIAN_POINT ( 'NONE',  ( 0.000000000000000000, 5.977523610840987267, 32.81826849749789687 ) ) ;
#10699 = FACE_OUTER_BOUND ( 'NONE', #13747, .T. ) ;
#10700 = CARTESIAN_POINT ( 'NONE',  ( -10.00000000000000000, 38.59999999999999432, 2.499999999999996003 ) ) ;
#10701 = CARTESIAN_POINT ( 'NONE',  ( -4.243569643749997233, -21.10823983395705383, -10.13570068892072840 ) ) ;
#10702 = ORIENTED_EDGE ( 'NONE', *, *, #11122, .F. ) ;
#10703 = LINE ( 'NONE', #10520, #1233 ) ;
#10704 = CARTESIAN_POINT ( 'NONE',  ( -10.00000000000000000, 34.19999999999999574, 2.499999999999996003 ) ) ;
#10705 = PRESENTATION_LAYER_ASSIGNMENT (  '', '', ( #5679 ) ) ;
#10706 = CARTESIAN_POINT ( 'NONE',  ( -2.055738996568313048, 33.24680007765648782, -1.423772053676023441 ) ) ;
#10707 = VERTEX_POINT ( 'NONE', #2535 ) ;
#10708 = CARTESIAN_POINT ( 'NONE',  ( 2.211161402132902243, 32.12180007765648071, 2.942372952327172442 ) ) ;
#10709 = CARTESIAN_POINT ( 'NONE',  ( 3.061616997868382648E-16, 3.000000000000000000, -2.499999999999999556 ) ) ;
#10710 = DIRECTION ( 'NONE',  ( -0.000000000000000000, -1.000000000000000000, -0.000000000000000000 ) ) ;
#10711 = ORIENTED_EDGE ( 'NONE', *, *, #5591, .T. ) ;
#10712 = VECTOR ( 'NONE', #15805, 1000.000000000000000 ) ;
#10713 = CARTESIAN_POINT ( 'NONE',  ( 4.243569643750003451, -20.19410238852258743, -8.830177118335141628 ) ) ;
#10714 = ADVANCED_FACE ( 'NONE', ( #11459 ), #11043, .T. ) ;
#10715 = CARTESIAN_POINT ( 'NONE',  ( 0.05938372350927906274, 22.37180007765648071, 3.680117784833935701 ) ) ;
#10716 = AXIS2_PLACEMENT_3D ( 'NONE', #15221, #3983, #16519 ) ;
#10717 =( BOUNDED_CURVE ( )  B_SPLINE_CURVE ( 2, ( #15017, #12212, #10917, #17897, #3693, #1286, #15199, #1098, #12478 ),
 .UNSPECIFIED., .F., .T. ) 
 B_SPLINE_CURVE_WITH_KNOTS ( ( 3, 2, 2, 2, 3 ),
 ( 0.09482758620689656082, 0.09770114942528736190, 0.1034482758620689641, 0.1091954022988505801, 0.1120689655172413812 ),
 .UNSPECIFIED. ) 
 CURVE ( )  GEOMETRIC_REPRESENTATION_ITEM ( )  RATIONAL_B_SPLINE_CURVE ( ( 0.9330127018922194093, 0.9330127018922195203, 1.000000000000000000, 0.8660254037844387076, 1.000000000000000000, 0.8660254037844387076, 1.000000000000000000, 0.9330127018922194093, 0.9330127018922194093 ) ) 
 REPRESENTATION_ITEM ( '' )  );
#10718 = ORIENTED_EDGE ( 'NONE', *, *, #11537, .F. ) ;
#10719 = DIRECTION ( 'NONE',  ( -0.000000000000000000, 1.000000000000000000, -0.000000000000000000 ) ) ;
#10720 = CARTESIAN_POINT ( 'NONE',  ( 4.000000000000000000, -1.759474945355381292, 3.047500000000002540 ) ) ;
#10721 = CARTESIAN_POINT ( 'NONE',  ( -1.098144841579475894, -23.88987786432218385, -16.68580408662743864 ) ) ;
#10722 = CARTESIAN_POINT ( 'NONE',  ( 9.175740695410866010, -10.00000000000000178, -2.948767207631089793 ) ) ;
#10723 = CARTESIAN_POINT ( 'NONE',  ( 4.000000000000003553, -22.71293939747845769, -12.18227696742093791 ) ) ;
#10724 = CARTESIAN_POINT ( 'NONE',  ( -4.243569643750005227, -22.53027904986517527, -3.623602937346249497 ) ) ;
#10725 = ORIENTED_EDGE ( 'NONE', *, *, #9426, .T. ) ;
#10726 = DIRECTION ( 'NONE',  ( -1.000000000000000000, 0.000000000000000000, 4.336808689942021680E-16 ) ) ;
#10727 = AXIS2_PLACEMENT_3D ( 'NONE', #3403, #7466, #5982 ) ;
#10728 = CARTESIAN_POINT ( 'NONE',  ( -5.279047395330986450E-15, -27.24820807026550540, -6.580358161266123496 ) ) ;
#10729 = AXIS2_PLACEMENT_3D ( 'NONE', #10460, #6291, #458 ) ;
#10730 = CARTESIAN_POINT ( 'NONE',  ( -2.798362969681365886, 35.24680007765648071, 2.102939460078824929 ) ) ;
#10731 = ORIENTED_EDGE ( 'NONE', *, *, #1738, .F. ) ;
#10732 = ORIENTED_EDGE ( 'NONE', *, *, #4053, .F. ) ;
#10733 = DIRECTION ( 'NONE',  ( -3.373073425510457965E-16, 0.000000000000000000, -1.000000000000000000 ) ) ;
#10734 = EDGE_CURVE ( 'NONE', #8825, #4590, #12498, .T. ) ;
#10735 = SURFACE_SIDE_STYLE ('',( #13428 ) ) ;
#10736 = CARTESIAN_POINT ( 'NONE',  ( -4.518350579753602325, 34.37819992234354771, 1.405661355842794391 ) ) ;
#10737 = CARTESIAN_POINT ( 'NONE',  ( -2.211161402132838738, 34.12819992234354771, 2.942372952327218183 ) ) ;
#10738 = EDGE_CURVE ( 'NONE', #5725, #2406, #13737, .T. ) ;
#10739 = CARTESIAN_POINT ( 'NONE',  ( 1.497042530366522461, 28.62819992234355126, 2.161531897785029965 ) ) ;
#10740 = VERTEX_POINT ( 'NONE', #9646 ) ;
#10741 = CARTESIAN_POINT ( 'NONE',  ( -1.336863392178478716, 19.99680007765647716, 4.297206761780677731 ) ) ;
#10742 = CARTESIAN_POINT ( 'NONE',  ( -4.000000000000000888, -20.36739408704506715, -4.806173200523589095 ) ) ;
#10743 = ORIENTED_EDGE ( 'NONE', *, *, #7031, .T. ) ;
#10744 = VECTOR ( 'NONE', #1197, 1000.000000000000000 ) ;
#10745 = DIRECTION ( 'NONE',  ( -0.000000000000000000, -1.000000000000000000, -0.000000000000000000 ) ) ;
#10746 = AXIS2_PLACEMENT_3D ( 'NONE', #668, #11867, #2066 ) ;
#10747 = CARTESIAN_POINT ( 'NONE',  ( 1.135272562821090458, 39.74680007765648071, 3.311245368580554072 ) ) ;
#10748 = CARTESIAN_POINT ( 'NONE',  ( 1.071796769724500109, -22.07091849049882271, -14.21284536423708467 ) ) ;
#10749 = CARTESIAN_POINT ( 'NONE',  ( 2.121784821874994176, -22.92074116793234140, -2.045495577151484223 ) ) ;
#10750 = CARTESIAN_POINT ( 'NONE',  ( 4.243569643750000786, -24.02932114822622722, -10.03594703378452024 ) ) ;
#10751 = CARTESIAN_POINT ( 'NONE',  ( -1.657547274258957426, -30.02955948770827277, -12.21735830786932731 ) ) ;
#10752 = ORIENTED_EDGE ( 'NONE', *, *, #14417, .F. ) ;
#10753 = CARTESIAN_POINT ( 'NONE',  ( -3.132887738848217918, -10.75727755901226956, 20.85177242120514407 ) ) ;
#10754 = AXIS2_PLACEMENT_3D ( 'NONE', #18243, #5513, #4214 ) ;
#10755 = CARTESIAN_POINT ( 'NONE',  ( -1.071796769724486786, -19.46677112548146127, -10.49373749562478153 ) ) ;
#10756 = CARTESIAN_POINT ( 'NONE',  ( -2.121784821874996396, -23.51396284310121487, -15.70717426502434044 ) ) ;
#10757 = VERTEX_POINT ( 'NONE', #9468 ) ;
#10758 = VECTOR ( 'NONE', #12686, 1000.000000000000000 ) ;
#10759 = CARTESIAN_POINT ( 'NONE',  ( -0.05938372350920063936, 38.87819992234354771, 3.680117784833935701 ) ) ;
#10760 = DIRECTION ( 'NONE',  ( -1.000000000000000000, 0.000000000000000000, 0.000000000000000000 ) ) ;
#10761 = EDGE_CURVE ( 'NONE', #278, #15565, #7289, .T. ) ;
#10762 = CARTESIAN_POINT ( 'NONE',  ( 2.121784821874994176, -23.43695996064828435, -2.782732417011581028 ) ) ;
#10763 = CARTESIAN_POINT ( 'NONE',  ( 1.497042530366477164, 28.87180007765648426, -2.161531897785062384 ) ) ;
#10764 = CARTESIAN_POINT ( 'NONE',  ( 2.829195390882724759, 15.37819992234354594, -3.793023760679264278 ) ) ;
#10765 = CARTESIAN_POINT ( 'NONE',  ( -3.999999999999997335, -22.88501232838376254, -12.42802258070763877 ) ) ;
#10766 = ORIENTED_EDGE ( 'NONE', *, *, #4215, .F. ) ;
#10767 = CARTESIAN_POINT ( 'NONE',  ( -4.243569643749997233, -18.81751894128008118, -6.864212212041558736 ) ) ;
#10768 = CARTESIAN_POINT ( 'NONE',  ( -0.05938372350928957516, 38.62180007765647360, -4.731580009072201776 ) ) ;
#10769 = CIRCLE ( 'NONE', #2790, 0.9999999999999991118 ) ;
#10770 = SHAPE_REPRESENTATION ( 'socket head cap screw_iso_ISO 4762 M8 x 12 - 12N', ( #16940 ), #3923 ) ;
#10771 = CARTESIAN_POINT ( 'NONE',  ( -1.734723475976807094E-15, 43.00000000000000000, -2.500000000000000000 ) ) ;
#10772 = CARTESIAN_POINT ( 'NONE',  ( -8.500000000000005329, 10.00000000000000000, 22.50000000000000000 ) ) ;
#10773 = CARTESIAN_POINT ( 'NONE',  ( -5.577813053751546416E-15, -25.96698683212770931, -5.829433235496615850 ) ) ;
#10774 = VERTEX_POINT ( 'NONE', #5816 ) ;
#10775 = ORIENTED_EDGE ( 'NONE', *, *, #2547, .F. ) ;
#10776 = CARTESIAN_POINT ( 'NONE',  ( -2.115076519116362519, 17.62180007765647716, 3.012182706137107147 ) ) ;
#10777 = CARTESIAN_POINT ( 'NONE',  ( -3.706921591972381904E-14, -18.25227819420489439, -8.759261836619732122 ) ) ;
#10778 = CARTESIAN_POINT ( 'NONE',  ( 1.533898589781675205E-14, -27.45111586048108521, -7.948989149087622330 ) ) ;
#10779 = ORIENTED_EDGE ( 'NONE', *, *, #9600, .F. ) ;
#10780 = CARTESIAN_POINT ( 'NONE',  ( -2.500000000000001332, 39.50319992234355482, -0.05647727720530596601 ) ) ;
#10781 = CARTESIAN_POINT ( 'NONE',  ( 2.121784821874994176, -26.79238211330187625, -7.574771876102201595 ) ) ;
#10782 = CARTESIAN_POINT ( 'NONE',  ( -3.481649420246369697, 22.87180007765647360, 1.193696214020542490 ) ) ;
#10783 = CARTESIAN_POINT ( 'NONE',  ( -3.604268994871580034, -29.27461685626023424, -13.12700564398634917 ) ) ;
#10784 = CARTESIAN_POINT ( 'NONE',  ( -1.999999999999996225, -21.18631794911805599, -12.01519454243453211 ) ) ;
#10785 = CARTESIAN_POINT ( 'NONE',  ( 2.121784821874994176, -27.85708337327849549, -9.095322858313648950 ) ) ;
#10786 = CIRCLE ( 'NONE', #11366, 0.9999999999999991118 ) ;
#10787 = ADVANCED_FACE ( 'NONE', ( #11555 ), #16636, .F. ) ;
#10788 = EDGE_CURVE ( 'NONE', #7842, #17988, #5517, .T. ) ;
#10789 = FACE_OUTER_BOUND ( 'NONE', #11998, .T. ) ;
#10791 = CARTESIAN_POINT ( 'NONE',  ( 0.05938372350929014415, 24.87180007765647716, 4.731580009072201776 ) ) ;
#10790 =( REPRESENTATION_RELATIONSHIP ('NONE','NONE', #15868, #1416 ) REPRESENTATION_RELATIONSHIP_WITH_TRANSFORMATION ( #6812 )SHAPE_REPRESENTATION_RELATIONSHIP( ) );
#10792 = EDGE_CURVE ( 'NONE', #11376, #14634, #516, .T. ) ;
#10793 = CARTESIAN_POINT ( 'NONE',  ( -5.577813053751546416E-15, -23.38589286854802296, -2.143249036196138047 ) ) ;
#10794 = CARTESIAN_POINT ( 'NONE',  ( -8.500000000000010658, 13.00000000000000000, 20.49999999999998934 ) ) ;
#10795 = CARTESIAN_POINT ( 'NONE',  ( 4.243569643749996345, -23.96063528801558462, -5.666363347791923744 ) ) ;
#10796 = ORIENTED_EDGE ( 'NONE', *, *, #8082, .T. ) ;
#10797 = DIRECTION ( 'NONE',  ( -1.000000000000000000, -0.000000000000000000, -0.000000000000000000 ) ) ;
#10798 = DIRECTION ( 'NONE',  ( -0.000000000000000000, -0.5000000000000001110, 0.8660254037844385966 ) ) ;
#10799 = DIRECTION ( 'NONE',  ( -1.000000000000000000, 0.000000000000000000, 4.336808689942021680E-16 ) ) ;
#10800 = EDGE_CURVE ( 'NONE', #3808, #6738, #4332, .T. ) ;
#10801 = CARTESIAN_POINT ( 'NONE',  ( -2.500000000000001332, 27.99680007765648426, 0.05647727720535858364 ) ) ;
#10802 = DIRECTION ( 'NONE',  ( -1.000000000000000000, 0.000000000000000000, 0.000000000000000000 ) ) ;
#10803 = CARTESIAN_POINT ( 'NONE',  ( 2.115076519116362963, 31.37180007765647716, -3.012182706137107591 ) ) ;
#10804 = CARTESIAN_POINT ( 'NONE',  ( -5.577813053751546416E-15, -23.32136551875358776, -2.051094430206859887 ) ) ;
#10805 = PLANE ( 'NONE',  #1296 ) ;
#10806 = EDGE_CURVE ( 'NONE', #11197, #10707, #15654, .T. ) ;
#10807 = VERTEX_POINT ( 'NONE', #18124 ) ;
#10808 = CARTESIAN_POINT ( 'NONE',  ( -2.121784821874996396, -18.35177491594184218, -8.334805866423387499 ) ) ;
#10809 = CARTESIAN_POINT ( 'NONE',  ( 3.481649420246369697, 26.62180007765648071, -1.193696214020541824 ) ) ;
#10810 = VERTEX_POINT ( 'NONE', #14262 ) ;
#10811 = CARTESIAN_POINT ( 'NONE',  ( 1.071796769724504328, -25.11660459254052924, -4.614961535061283371 ) ) ;
#10812 = CYLINDRICAL_SURFACE ( 'NONE', #17777, 0.9999999999999991118 ) ;
#10813 = CARTESIAN_POINT ( 'NONE',  ( -0.5794581908436565731, -23.80035312255054691, -16.75679979387895102 ) ) ;
#10814 = CARTESIAN_POINT ( 'NONE',  ( 6.428571428571432378, -11.73421655796352248, 14.25837509840158290 ) ) ;
#10815 = CARTESIAN_POINT ( 'NONE',  ( -31.74999999999995737, 0.000000000000000000, 0.000000000000000000 ) ) ;
#10816 = CARTESIAN_POINT ( 'NONE',  ( 2.121784821874994176, -23.46922363519303190, -2.828809719502837439 ) ) ;
#10817 = ORIENTED_EDGE ( 'NONE', *, *, #477, .T. ) ;
#10818 = DIRECTION ( 'NONE',  ( -0.000000000000000000, -1.000000000000000000, -0.000000000000000000 ) ) ;
#10819 = CARTESIAN_POINT ( 'NONE',  ( -4.000000000000000888, -23.27112479677715839, -8.953130425743392351 ) ) ;
#10820 = CARTESIAN_POINT ( 'NONE',  ( 2.115076519116362963, 33.87180007765648071, -3.012182706137107147 ) ) ;
#10821 = EDGE_LOOP ( 'NONE', ( #14972, #2539, #12113, #14563 ) ) ;
#10822 = ORIENTED_EDGE ( 'NONE', *, *, #17154, .T. ) ;
#10823 = CARTESIAN_POINT ( 'NONE',  ( 0.000000000000000000, 4.000000000000007105, 4.000000000000000000 ) ) ;
#10824 = CARTESIAN_POINT ( 'NONE',  ( 3.607379964056363075, 36.00319992234354771, 2.690724712371229010 ) ) ;
#10825 = CARTESIAN_POINT ( 'NONE',  ( 7.999999999999998224, 13.00000000000000178, -2.500000000000003109 ) ) ;
#10826 = CARTESIAN_POINT ( 'NONE',  ( 1.497042530366522461, 31.12819992234354416, 2.161531897785029965 ) ) ;
#10827 =( BOUNDED_CURVE ( )  B_SPLINE_CURVE ( 2, ( #3529, #17555, #5000, #9080, #9175, #13159, #3439, #10748, #14855 ),
 .UNSPECIFIED., .F., .F. ) 
 B_SPLINE_CURVE_WITH_KNOTS ( ( 3, 2, 2, 2, 3 ),
 ( 0.2327586206896551657, 0.2356321839080459668, 0.2413793103448275967, 0.2471264367816091989, 0.2500000000000000000 ),
 .UNSPECIFIED. ) 
 CURVE ( )  GEOMETRIC_REPRESENTATION_ITEM ( )  RATIONAL_B_SPLINE_CURVE ( ( 0.9330127018922194093, 0.9330127018922194093, 1.000000000000000000, 0.8660254037844387076, 1.000000000000000000, 0.8660254037844387076, 1.000000000000000000, 0.9330127018922197424, 0.9330127018922194093 ) ) 
 REPRESENTATION_ITEM ( '' )  );
#10828 = ORIENTED_EDGE ( 'NONE', *, *, #16261, .F. ) ;
#10829 = CARTESIAN_POINT ( 'NONE',  ( 4.499999999999999112, 29.24680007765647716, -0.05647727720537982360 ) ) ;
#10830 = AXIS2_PLACEMENT_3D ( 'NONE', #12828, #224, #5875 ) ;
#10831 = CARTESIAN_POINT ( 'NONE',  ( 2.000000000000004441, -17.35769523647485713, -6.547354646805487732 ) ) ;
#10832 = ORIENTED_EDGE ( 'NONE', *, *, #8067, .F. ) ;
#10833 = CARTESIAN_POINT ( 'NONE',  ( 15.00000000000000355, 10.00000000000000000, -30.00000000000000000 ) ) ;
#10834 = CARTESIAN_POINT ( 'NONE',  ( 2.798362969681366330, 36.49680007765648071, -2.102939460078824929 ) ) ;
#10835 = CARTESIAN_POINT ( 'NONE',  ( 1.300000000000000044, 1.443375672974065216, 7.222237291452134449E-31 ) ) ;
#10836 = CARTESIAN_POINT ( 'NONE',  ( 1.300000000000000044, 0.7216878364870329410, 1.249999999999999778 ) ) ;
#10837 = CARTESIAN_POINT ( 'NONE',  ( -4.243569643750000786, -24.41648524276317289, -10.58887466367959540 ) ) ;
#10838 = CARTESIAN_POINT ( 'NONE',  ( 19.30950000000002120, 0.000000000000000000, 4.000000000000000888 ) ) ;
#10839 = EDGE_LOOP ( 'NONE', ( #15430, #3697, #17183, #10029 ) ) ;
#10840 = TOROIDAL_SURFACE ( 'NONE', #9372, 2.200000000000000178, 0.2000000000000000111 ) ;
#10841 = DIRECTION ( 'NONE',  ( -0.000000000000000000, -1.000000000000000000, -0.000000000000000000 ) ) ;
#10842 = DIRECTION ( 'NONE',  ( -0.000000000000000000, -0.000000000000000000, 1.000000000000000000 ) ) ;
#10843 = CARTESIAN_POINT ( 'NONE',  ( -3.706921591972381904E-14, -18.76849698692083379, -9.496498676479825818 ) ) ;
#10844 = CARTESIAN_POINT ( 'NONE',  ( -4.243569643750000786, -26.73946980998488954, -13.90644044305002502 ) ) ;
#10845 = VERTEX_POINT ( 'NONE', #1565 ) ;
#10846 = CARTESIAN_POINT ( 'NONE',  ( -3.518350579753605434, 36.87819992234354771, 1.080741659609877781 ) ) ;
#10847 = FACE_BOUND ( 'NONE', #7969, .T. ) ;
#10848 = CARTESIAN_POINT ( 'NONE',  ( -2.121784821874996396, -17.02896425960724969, -6.445636464281891520 ) ) ;
#10849 = CARTESIAN_POINT ( 'NONE',  ( 1.989345975306426206, 26.49680007765648426, -1.515154207786343799 ) ) ;
#10850 = CARTESIAN_POINT ( 'NONE',  ( -3.607379964056363075, 27.25319992234354771, -2.690724712371229899 ) ) ;
#10851 = UNCERTAINTY_MEASURE_WITH_UNIT (LENGTH_MEASURE( 1.000000000000000082E-05 ), #8221, 'distance_accuracy_value', 'NONE');
#10852 = CARTESIAN_POINT ( 'NONE',  ( -4.000000000000004441, -26.36738592551932925, -9.348731678031116488 ) ) ;
#10853 = VERTEX_POINT ( 'NONE', #12858 ) ;
#10854 = CARTESIAN_POINT ( 'NONE',  ( -1.999999999999996225, -22.79950167706030228, -14.31905966800409402 ) ) ;
#10855 = EDGE_CURVE ( 'NONE', #5429, #10347, #165, .T. ) ;
#10856 = AXIS2_PLACEMENT_3D ( 'NONE', #5861, #11694, #17199 ) ;
#10857 = CARTESIAN_POINT ( 'NONE',  ( 0.05938372350929014415, 37.37180007765647360, 4.731580009072201776 ) ) ;
#10858 = CARTESIAN_POINT ( 'NONE',  ( 2.121784821875004390, -20.94362343770310986, -12.03634916655427922 ) ) ;
#10859 = EDGE_CURVE ( 'NONE', #9470, #11559, #330, .T. ) ;
#10860 = CARTESIAN_POINT ( 'NONE',  ( -1.071796769724496334, -28.75318954298976237, -9.808543083393779227 ) ) ;
#10861 = CARTESIAN_POINT ( 'NONE',  ( 4.299564228933482956E-15, -21.02695420434810814, -12.72190984986098172 ) ) ;
#10862 = CARTESIAN_POINT ( 'NONE',  ( -1.734723475976807094E-15, 23.19999999999999574, -2.500000000000000000 ) ) ;
#10863 = ORIENTED_EDGE ( 'NONE', *, *, #6381, .F. ) ;
#10864 = VERTEX_POINT ( 'NONE', #13045 ) ;
#10865 = DIRECTION ( 'NONE',  ( 3.469446951953612217E-16, -0.000000000000000000, 1.000000000000000000 ) ) ;
#10866 = CARTESIAN_POINT ( 'NONE',  ( -4.000000000000007105, 0.000000000000000000, 5.000000000000000888 ) ) ;
#10867 = CARTESIAN_POINT ( 'NONE',  ( 1.999999999999994449, -29.63624580000097097, -12.00398843855210629 ) ) ;
#10868 = DIRECTION ( 'NONE',  ( 1.000000000000000000, 0.000000000000000000, 0.000000000000000000 ) ) ;
#10869 = ORIENTED_EDGE ( 'NONE', *, *, #15402, .F. ) ;
#10870 = CARTESIAN_POINT ( 'NONE',  ( -2.481649420246391902, 34.62819992234354771, -0.8687765177875723666 ) ) ;
#10871 = CARTESIAN_POINT ( 'NONE',  ( -4.243569643750005227, -25.59532813161604636, -8.000946674015564142 ) ) ;
#10872 = CARTESIAN_POINT ( 'NONE',  ( 3.500000000000000444, 31.74680007765647716, -0.05647727720536935281 ) ) ;
#10873 = CARTESIAN_POINT ( 'NONE',  ( -3.518350579753605434, 29.37819992234354416, 1.080741659609877781 ) ) ;
#10874 = DIRECTION ( 'NONE',  ( -0.000000000000000000, -0.5735764363510414965, -0.8191520442889950182 ) ) ;
#10875 = CARTESIAN_POINT ( 'NONE',  ( 4.243569643750000786, -27.11050206724947742, -14.43632942169946531 ) ) ;
#10876 = CARTESIAN_POINT ( 'NONE',  ( -2.121784821875005722, -26.86766402057294556, -7.682285581915135886 ) ) ;
#10877 = SHAPE_REPRESENTATION ( 'Coil Housing', ( #16940 ), #16347 ) ;
#10878 = AXIS2_PLACEMENT_3D ( 'NONE', #9715, #9896, #11284 ) ;
#10879 = AXIS2_PLACEMENT_3D ( 'NONE', #5884, #4678, #236 ) ;
#10880 = CARTESIAN_POINT ( 'NONE',  ( -8.500000000000005329, 0.000000000000000000, -18.49999999999999645 ) ) ;
#10881 = CARTESIAN_POINT ( 'NONE',  ( 1.444289557196047680, 24.74680007765647716, 4.262301884875704161 ) ) ;
#10882 = DIRECTION ( 'NONE',  ( -1.000000000000000000, 0.000000000000000000, 0.000000000000000000 ) ) ;
#10883 =( GEOMETRIC_REPRESENTATION_CONTEXT ( 3 ) GLOBAL_UNCERTAINTY_ASSIGNED_CONTEXT ( ( #12666 ) ) GLOBAL_UNIT_ASSIGNED_CONTEXT ( ( #17600, #9124, #9736 ) ) REPRESENTATION_CONTEXT ( 'NONE', 'WORKASPACE' ) );
#10884 = DIRECTION ( 'NONE',  ( 1.000000000000000000, 0.000000000000000000, -4.336808689942021680E-16 ) ) ;
#10885 = CARTESIAN_POINT ( 'NONE',  ( 4.730628863548789710E-15, -17.33754842334290913, -9.022085378453862603 ) ) ;
#10886 = ORIENTED_EDGE ( 'NONE', *, *, #12042, .F. ) ;
#10887 = FACE_BOUND ( 'NONE', #13354, .T. ) ;
#10888 = DIRECTION ( 'NONE',  ( -3.469446951953613696E-16, -0.000000000000000000, -1.000000000000000000 ) ) ;
#10889 = CARTESIAN_POINT ( 'NONE',  ( -0.05938372350926768989, 36.12180007765648071, -2.628655560595669183 ) ) ;
#10890 = CARTESIAN_POINT ( 'NONE',  ( 2.000000000000004441, -20.51953534256492162, -11.06293029195533784 ) ) ;
#10891 = CARTESIAN_POINT ( 'NONE',  ( -2.864755990943265829, 38.24680007765647360, -2.011557305968488141 ) ) ;
#10892 = FACE_OUTER_BOUND ( 'NONE', #3187, .T. ) ;
#10893 = ADVANCED_FACE ( 'NONE', ( #13419 ), #10353, .T. ) ;
#10894 = APPLICATION_PROTOCOL_DEFINITION ( 'draft international standard', 'automotive_design', 1998, #5355 ) ;
#10895 = ADVANCED_FACE ( 'NONE', ( #4522 ), #3478, .T. ) ;
#10896 = CARTESIAN_POINT ( 'NONE',  ( -2.417956891975437728, 15.00000000000001066, -3.010107623731891113 ) ) ;
#10897 = EDGE_CURVE ( 'NONE', #4661, #15374, #7610, .T. ) ;
#10898 = VERTEX_POINT ( 'NONE', #1946 ) ;
#10899 = CARTESIAN_POINT ( 'NONE',  ( 4.730628863548789710E-15, -16.85359330517172083, -8.330925841085024430 ) ) ;
#10900 = CARTESIAN_POINT ( 'NONE',  ( -0.05938372350927861171, 23.62180007765647005, -3.680117784833935701 ) ) ;
#10901 = ORIENTED_EDGE ( 'NONE', *, *, #12084, .F. ) ;
#10902 = LINE ( 'NONE', #16393, #17077 ) ;
#10903 = CARTESIAN_POINT ( 'NONE',  ( 4.243569643750000786, -27.09437022997710187, -14.41329077045383578 ) ) ;
#10904 = AXIS2_PLACEMENT_3D ( 'NONE', #14628, #13209, #9228 ) ;
#10905 = DIRECTION ( 'NONE',  ( 0.000000000000000000, 0.000000000000000000, -1.000000000000000000 ) ) ;
#10906 =( GEOMETRIC_REPRESENTATION_CONTEXT ( 3 ) GLOBAL_UNCERTAINTY_ASSIGNED_CONTEXT ( ( #14002 ) ) GLOBAL_UNIT_ASSIGNED_CONTEXT ( ( #2985, #480, #3358 ) ) REPRESENTATION_CONTEXT ( 'NONE', 'WORKASPACE' ) );
#10907 = CARTESIAN_POINT ( 'NONE',  ( -1.999999999999996225, -19.63766157097024490, -9.803484022854247470 ) ) ;
#10909 = CARTESIAN_POINT ( 'NONE',  ( -3.999999999999997335, -19.01337138301423124, -6.898746281756922727 ) ) ;
#10908 = CIRCLE ( 'NONE', #9995, 0.9999999999999991118 ) ;
#10910 = CARTESIAN_POINT ( 'NONE',  ( 2.121784821875004390, -23.00849860856686036, -14.98529652599465933 ) ) ;
#10911 = ORIENTED_EDGE ( 'NONE', *, *, #16258, .F. ) ;
#10912 = DIRECTION ( 'NONE',  ( -1.000000000000000000, -0.000000000000000000, -0.000000000000000000 ) ) ;
#10913 = CARTESIAN_POINT ( 'NONE',  ( 2.000000000000004441, -18.71276956805914082, -8.482601352445005460 ) ) ;
#10914 = CARTESIAN_POINT ( 'NONE',  ( 1.027846397803542144, 36.24680007765648071, -3.346150245485522312 ) ) ;
#10915 = ORIENTED_EDGE ( 'NONE', *, *, #15904, .F. ) ;
#10916 = ORIENTED_EDGE ( 'NONE', *, *, #17852, .T. ) ;
#10917 = CARTESIAN_POINT ( 'NONE',  ( 1.999999999999994449, -29.12002700728503513, -11.26675159869200904 ) ) ;
#10918 = CARTESIAN_POINT ( 'NONE',  ( -2.733110507866328476, 37.37819992234354771, -3.862833514489096398 ) ) ;
#10919 = CARTESIAN_POINT ( 'NONE',  ( 4.000000000000000000, 0.000000000000000000, 0.000000000000000000 ) ) ;
#10920 = EDGE_CURVE ( 'NONE', #11829, #94, #8479, .T. ) ;
#10921 = CARTESIAN_POINT ( 'NONE',  ( 2.055738996568281518, 30.50319992234354771, -1.423772053676066518 ) ) ;
#10922 = VERTEX_POINT ( 'NONE', #11739 ) ;
#10923 = CARTESIAN_POINT ( 'NONE',  ( 2.121784821875004390, -22.52454349039567205, -14.29413698862582294 ) ) ;
#10924 = CARTESIAN_POINT ( 'NONE',  ( 3.673772985318219053, 26.99680007765647716, 2.599342558260951730 ) ) ;
#10925 = CARTESIAN_POINT ( 'NONE',  ( 4.000000000000000888, -20.49644878522406088, -4.990482410488609410 ) ) ;
#10926 = ORIENTED_EDGE ( 'NONE', *, *, #11344, .F. ) ;
#10927 = CARTESIAN_POINT ( 'NONE',  ( -1.734723475976807094E-15, 23.19999999999999574, -2.500000000000000000 ) ) ;
#10928 = ADVANCED_BREP_SHAPE_REPRESENTATION ( '', ( #8321, #16940 ), #8637 ) ;
#10929 = DIRECTION ( 'NONE',  ( 0.000000000000000000, 0.000000000000000000, -1.000000000000000000 ) ) ;
#10930 = CARTESIAN_POINT ( 'NONE',  ( -2.121784821874996396, -17.28707365596521939, -6.814254884211938368 ) ) ;
#10931 = CARTESIAN_POINT ( 'NONE',  ( -4.243569643750005227, -24.85326361708688836, -6.941168716716678233 ) ) ;
#10932 = AXIS2_PLACEMENT_3D ( 'NONE', #1300, #15486, #1114 ) ;
#10933 = ADVANCED_FACE ( 'NONE', ( #17628 ), #18006, .T. ) ;
#10934 = DIRECTION ( 'NONE',  ( -0.000000000000000000, -0.5735764363510414965, -0.8191520442889950182 ) ) ;
#10935 = ORIENTED_EDGE ( 'NONE', *, *, #16832, .T. ) ;
#10936 = CARTESIAN_POINT ( 'NONE',  ( 4.000000000000000888, -23.91639828767208442, -9.874676475568506362 ) ) ;
#10937 = DIRECTION ( 'NONE',  ( 0.000000000000000000, 0.8191520442889952403, -0.5735764363510413855 ) ) ;
#10938 = DIRECTION ( 'NONE',  ( -0.5000000000000042188, 1.060575238724903710E-16, -0.8660254037844361541 ) ) ;
#10939 = ORIENTED_EDGE ( 'NONE', *, *, #11082, .F. ) ;
#10940 = CARTESIAN_POINT ( 'NONE',  ( -1.135272562821019626, 34.00319992234354771, 3.311245368580577164 ) ) ;
#10941 = CARTESIAN_POINT ( 'NONE',  ( 3.481649420246395010, 20.87819992234354416, 1.193696214020467439 ) ) ;
#10942 = CARTESIAN_POINT ( 'NONE',  ( 2.121784821874994176, -23.17885056429031465, -2.414113997081532847 ) ) ;
#10943 = CARTESIAN_POINT ( 'NONE',  ( 0.8262555684461332373, 29.74680007765648426, 2.360188852285403982 ) ) ;
#10944 = CARTESIAN_POINT ( 'NONE',  ( 2.733110507866328920, 26.12819992234354416, 3.862833514489095510 ) ) ;
#10945 = CARTESIAN_POINT ( 'NONE',  ( -4.000000000000004441, -27.39982351095120450, -10.82320535775130566 ) ) ;
#10946 = ORIENTED_EDGE ( 'NONE', *, *, #238, .T. ) ;
#10947 = AXIS2_PLACEMENT_3D ( 'NONE', #10137, #15818, #142 ) ;
#10948 = CARTESIAN_POINT ( 'NONE',  ( -4.243569643750005227, -22.27216965350720201, -3.254984517416200873 ) ) ;
#10949 = CARTESIAN_POINT ( 'NONE',  ( 3.673772985318219053, 36.99680007765647360, 2.599342558260951730 ) ) ;
#10950 = DIRECTION ( 'NONE',  ( 0.000000000000000000, 0.000000000000000000, 1.000000000000000000 ) ) ;
#10951 = CARTESIAN_POINT ( 'NONE',  ( 4.243569643750000786, -24.77138566275538523, -11.09572499108340793 ) ) ;
#10952 = CARTESIAN_POINT ( 'NONE',  ( -2.000000000000005773, -28.84040849385894845, -10.86741497609436280 ) ) ;
#10953 = CARTESIAN_POINT ( 'NONE',  ( -3.706921591972381904E-14, -17.99416879784692469, -8.390643416689682610 ) ) ;
#10954 = AXIS2_PLACEMENT_3D ( 'NONE', #14507, #11700, #17769 ) ;
#10955 = CARTESIAN_POINT ( 'NONE',  ( -4.000000000000004441, -25.14136629352392660, -7.597794184370154191 ) ) ;
#10956 = ORIENTED_EDGE ( 'NONE', *, *, #12476, .F. ) ;
#10957 = ORIENTED_EDGE ( 'NONE', *, *, #7103, .F. ) ;
#10958 = CARTESIAN_POINT ( 'NONE',  ( -1.135272562821090014, 15.99680007765647716, -3.311245368580554072 ) ) ;
#10959 = FACE_OUTER_BOUND ( 'NONE', #2891, .T. ) ;
#10960 = EDGE_CURVE ( 'NONE', #2307, #1671, #5414, .T. ) ;
#10961 = DIRECTION ( 'NONE',  ( -0.5000000000000061062, 1.060575238724902601E-16, -0.8660254037844351549 ) ) ;
#10962 = CARTESIAN_POINT ( 'NONE',  ( 7.143939857752706679, -13.70057337075539117, 0.6943083681407321572 ) ) ;
#10963 = ORIENTED_EDGE ( 'NONE', *, *, #12653, .T. ) ;
#10964 = VECTOR ( 'NONE', #6419, 1000.000000000000114 ) ;
#10965 = CARTESIAN_POINT ( 'NONE',  ( 2.500000000000001332, 33.25319992234354771, 0.05647727720530566764 ) ) ;
#10966 = CARTESIAN_POINT ( 'NONE',  ( 2.121784821874994176, -27.05049150965984595, -7.943390296032248443 ) ) ;
#10967 = CARTESIAN_POINT ( 'NONE',  ( -3.518350579753630747, 33.12180007765646650, -1.080741659609802729 ) ) ;
#10968 = EDGE_CURVE ( 'NONE', #18352, #3556, #7383, .T. ) ;
#10969 = CARTESIAN_POINT ( 'NONE',  ( -1.027846397803611866, 25.00319992234354416, -3.346150245485499219 ) ) ;
#10970 = DIRECTION ( 'NONE',  ( 0.000000000000000000, 0.8191520442889952403, -0.5735764363510413855 ) ) ;
#10971 = EDGE_CURVE ( 'NONE', #7464, #16667, #18313, .T. ) ;
#10972 = PLANE ( 'NONE',  #7868 ) ;
#10973 = EDGE_CURVE ( 'NONE', #2986, #15033, #14737, .T. ) ;
#10974 = CARTESIAN_POINT ( 'NONE',  ( 4.243569643749996345, -25.79966473706612007, -8.292769589793513418 ) ) ;
#10975 = TOROIDAL_SURFACE ( 'NONE', #4174, 9.000000000000001776, 0.9999999999999991118 ) ;
#10976 = PLANE ( 'NONE',  #12636 ) ;
#10977 = CARTESIAN_POINT ( 'NONE',  ( 1.444289557196047680, 22.24680007765647716, 4.262301884875704161 ) ) ;
#10978 = DIRECTION ( 'NONE',  ( -0.000000000000000000, -1.000000000000000000, -0.000000000000000000 ) ) ;
#10979 = CARTESIAN_POINT ( 'NONE',  ( 4.000000000000000000, 3.518949890710770134, -4.119968255444916849E-15 ) ) ;
#10980 = CARTESIAN_POINT ( 'NONE',  ( -4.243569643749997233, -20.07580224852517858, -8.661227009200541005 ) ) ;
#10981 = CARTESIAN_POINT ( 'NONE',  ( 1.300000000000000044, -1.443375672974064328, 2.168404344971008868E-16 ) ) ;
#10982 = CARTESIAN_POINT ( 'NONE',  ( -1.734723475976807094E-15, 38.59999999999999432, -10.50000000000000178 ) ) ;
#10983 = CARTESIAN_POINT ( 'NONE',  ( -2.518350579753628526, 35.62180007765647360, -0.7558219633769075463 ) ) ;
#10984 = FACE_OUTER_BOUND ( 'NONE', #2728, .T. ) ;
#10985 = CARTESIAN_POINT ( 'NONE',  ( 0.05938372350927906967, 37.37180007765647360, 3.680117784833935701 ) ) ;
#10986 = CARTESIAN_POINT ( 'NONE',  ( 0.000000000000000000, 15.00000000000000355, 5.000000000000000000 ) ) ;
#10987 = CARTESIAN_POINT ( 'NONE',  ( 0.000000000000000000, 5.977523610840987267, 32.81826849749789687 ) ) ;
#10988 = AXIS2_PLACEMENT_3D ( 'NONE', #5703, #2666, #5613 ) ;
#10989 = EDGE_LOOP ( 'NONE', ( #11048, #12089, #3042, #14264 ) ) ;
#10990 = CARTESIAN_POINT ( 'NONE',  ( -4.243569643750000786, -21.06106309010958100, -5.796835204588974833 ) ) ;
#10991 = CARTESIAN_POINT ( 'NONE',  ( -3.500000000000000444, 22.99680007765647716, 0.05647727720536892260 ) ) ;
#10992 = CARTESIAN_POINT ( 'NONE',  ( 0.000000000000000000, -21.06365275836378004, -18.87638460130267148 ) ) ;
#10993 = CARTESIAN_POINT ( 'NONE',  ( 2.121784821874994176, -29.63158547323952874, -11.62957449533272580 ) ) ;
#10994 = DIRECTION ( 'NONE',  ( -1.000000000000000000, 0.000000000000000000, 0.000000000000000000 ) ) ;
#10995 = STYLED_ITEM ( 'NONE', ( #17899 ), #18244 ) ;
#10996 = CARTESIAN_POINT ( 'NONE',  ( 3.999999999999993339, 0.000000000000000000, 30.00000000000000000 ) ) ;
#10997 = CARTESIAN_POINT ( 'NONE',  ( 4.243569643750000786, -27.12663390452184942, -14.45936807294509308 ) ) ;
#10998 = CARTESIAN_POINT ( 'NONE',  ( -4.243569643749997233, -23.68933379753673663, -13.82188488822120931 ) ) ;
#10999 = EDGE_CURVE ( 'NONE', #7792, #6738, #3508, .T. ) ;
#11000 = EDGE_LOOP ( 'NONE', ( #9276, #8806, #10572 ) ) ;
#11001 = PLANE ( 'NONE',  #627 ) ;
#11002 = CARTESIAN_POINT ( 'NONE',  ( 1.999999999999994449, -23.95783908012565888, -3.894383200091054320 ) ) ;
#11003 = CARTESIAN_POINT ( 'NONE',  ( -2.211161402132902243, 38.37180007765648071, -2.942372952327172886 ) ) ;
#11004 = ORIENTED_EDGE ( 'NONE', *, *, #1119, .F. ) ;
#11005 =( NAMED_UNIT ( * ) SI_UNIT ( $, .STERADIAN. ) SOLID_ANGLE_UNIT ( ) );
#11006 = CARTESIAN_POINT ( 'NONE',  ( -1.336863392178569088, 37.50319992234353350, -4.297206761780648421 ) ) ;
#11007 = CARTESIAN_POINT ( 'NONE',  ( -1.593127413382952939, 31.62819992234354416, 2.091722143975172532 ) ) ;
#11008 = VERTEX_POINT ( 'NONE', #14831 ) ;
#11009 = CARTESIAN_POINT ( 'NONE',  ( 4.730628863548789710E-15, -20.98334364689921827, -14.22882055996578998 ) ) ;
#11010 =( GEOMETRIC_REPRESENTATION_CONTEXT ( 3 ) GLOBAL_UNCERTAINTY_ASSIGNED_CONTEXT ( ( #16852 ) ) GLOBAL_UNIT_ASSIGNED_CONTEXT ( ( #3873, #828, #6292 ) ) REPRESENTATION_CONTEXT ( 'NONE', 'WORKASPACE' ) );
#11011 = CARTESIAN_POINT ( 'NONE',  ( 2.733110507866247652, 26.37180007765647716, -3.862833514489153686 ) ) ;
#11012 = CARTESIAN_POINT ( 'NONE',  ( 4.713407268011036227E-15, -16.64842020991469695, -7.547563884930901246 ) ) ;
#11013 = ORIENTED_EDGE ( 'NONE', *, *, #6552, .F. ) ;
#11014 = DIRECTION ( 'NONE',  ( 0.000000000000000000, 0.000000000000000000, -1.000000000000000000 ) ) ;
#11015 = EDGE_CURVE ( 'NONE', #15292, #9022, #2129, .T. ) ;
#11016 = DIRECTION ( 'NONE',  ( 0.000000000000000000, 0.000000000000000000, 1.000000000000000000 ) ) ;
#11017 = DIRECTION ( 'NONE',  ( 1.000000000000000000, 0.000000000000000000, 0.000000000000000000 ) ) ;
#11018 = ADVANCED_FACE ( 'NONE', ( #3768 ), #1186, .T. ) ;
#11019 = CARTESIAN_POINT ( 'NONE',  ( -2.121784821874996396, -20.41665008680558913, -11.28375322586376939 ) ) ;
#11020 = AXIS2_PLACEMENT_3D ( 'NONE', #346, #12933, #3124 ) ;
#11021 = EDGE_CURVE ( 'NONE', #1567, #5909, #7308, .T. ) ;
#11022 = CARTESIAN_POINT ( 'NONE',  ( -9.000000000000001776, 29.79999999999999716, 2.499999999999995559 ) ) ;
#11023 = EDGE_LOOP ( 'NONE', ( #12534, #9877, #18304, #17003 ) ) ;
#11024 = CARTESIAN_POINT ( 'NONE',  ( -5.279047395330986450E-15, -28.79686444841332360, -8.792068680846410800 ) ) ;
#11025 = CARTESIAN_POINT ( 'NONE',  ( 0.000000000000000000, 5.977523610840987267, 32.81826849749789687 ) ) ;
#11026 = CARTESIAN_POINT ( 'NONE',  ( 2.798362969681366330, 16.49680007765647716, -2.102939460078824929 ) ) ;
#11027 = CARTESIAN_POINT ( 'NONE',  ( 1.475796370471763337E-14, -21.86580974321645598, -13.91991971564040220 ) ) ;
#11028 = ORIENTED_EDGE ( 'NONE', *, *, #5704, .T. ) ;
#11029 = CARTESIAN_POINT ( 'NONE',  ( -2.211161402132839182, 36.62819992234354771, 2.942372952327218627 ) ) ;
#11030 = CARTESIAN_POINT ( 'NONE',  ( -1.135272562821019626, 21.50319992234354416, 3.311245368580577164 ) ) ;
#11031 = CARTESIAN_POINT ( 'NONE',  ( 4.713407268011036227E-15, -23.16568246865834979, -16.85517898917136748 ) ) ;
#11032 = CARTESIAN_POINT ( 'NONE',  ( 1.989345975306426206, 28.99680007765648071, -1.515154207786343799 ) ) ;
#11033 = AXIS2_PLACEMENT_3D ( 'NONE', #13579, #15270, #16474 ) ;
#11034 = CARTESIAN_POINT ( 'NONE',  ( 2.829195390882724759, 25.37819992234354416, -3.793023760679264278 ) ) ;
#11035 = VECTOR ( 'NONE', #14081, 1000.000000000000000 ) ;
#11036 = CARTESIAN_POINT ( 'NONE',  ( 4.713407268011036227E-15, -21.29438934435813024, -14.18269544367176316 ) ) ;
#11037 = EDGE_LOOP ( 'NONE', ( #4099, #10552, #8618, #466 ) ) ;
#11038 =( REPRESENTATION_RELATIONSHIP ('NONE','NONE', #15868, #1416 ) REPRESENTATION_RELATIONSHIP_WITH_TRANSFORMATION ( #9498 )SHAPE_REPRESENTATION_RELATIONSHIP( ) );
#11039 = CARTESIAN_POINT ( 'NONE',  ( -2.121784821875005722, -23.25413247156138397, -2.521627702894468470 ) ) ;
#11040 = CARTESIAN_POINT ( 'NONE',  ( -3.518350579753630747, 25.62180007765648071, -1.080741659609802729 ) ) ;
#11041 = DIRECTION ( 'NONE',  ( 0.000000000000000000, -1.000000000000000000, 0.000000000000000000 ) ) ;
#11042 = CARTESIAN_POINT ( 'NONE',  ( -4.243569643749998122, -20.33391164488314828, -9.029845429130586965 ) ) ;
#11043 = CYLINDRICAL_SURFACE ( 'NONE', #7910, 0.9999999999999991118 ) ;
#11044 = AXIS2_PLACEMENT_3D ( 'NONE', #805, #5057, #14536 ) ;
#11045 = CARTESIAN_POINT ( 'NONE',  ( 4.000000000000000000, 3.518949890710770134, -4.119968255444916849E-15 ) ) ;
#11046 = AXIS2_PLACEMENT_3D ( 'NONE', #9182, #17467, #2158 ) ;
#11047 = CARTESIAN_POINT ( 'NONE',  ( -8.500000000000005329, 0.000000000000000000, -20.49999999999999645 ) ) ;
#11048 = ORIENTED_EDGE ( 'NONE', *, *, #1677, .T. ) ;
#11049 = EDGE_LOOP ( 'NONE', ( #16313, #11112, #16810, #9776 ) ) ;
#11050 = DIRECTION ( 'NONE',  ( 1.000000000000000000, 0.000000000000000000, -4.336808689942021680E-16 ) ) ;
#11051 = DIRECTION ( 'NONE',  ( -0.000000000000000000, -0.5735764363510414965, -0.8191520442889950182 ) ) ;
#11052 = CARTESIAN_POINT ( 'NONE',  ( 3.999999999999996447, -23.50667344992347196, -5.263210858146513793 ) ) ;
#11053 =( NAMED_UNIT ( * ) SI_UNIT ( $, .STERADIAN. ) SOLID_ANGLE_UNIT ( ) );
#11054 = ORIENTED_EDGE ( 'NONE', *, *, #16322, .F. ) ;
#11055 = CARTESIAN_POINT ( 'NONE',  ( -0.8262555684460826111, 34.00319992234354771, 2.360188852285421302 ) ) ;
#11056 = CARTESIAN_POINT ( 'NONE',  ( -5.330712181944245322E-15, -27.81736316408238707, -6.902851464902143519 ) ) ;
#11057 = CARTESIAN_POINT ( 'NONE',  ( 3.481649420246369697, 34.12180007765648071, -1.193696214020541824 ) ) ;
#11058 = CARTESIAN_POINT ( 'NONE',  ( 3.518350579753605434, 23.12819992234354416, -1.080741659609877114 ) ) ;
#11059 = FACE_OUTER_BOUND ( 'NONE', #7125, .T. ) ;
#11060 = CARTESIAN_POINT ( 'NONE',  ( -9.000000000000001776, 40.79999999999999716, 2.499999999999995559 ) ) ;
#11061 = CIRCLE ( 'NONE', #1002, 3.309499999999999886 ) ;
#11062 = CARTESIAN_POINT ( 'NONE',  ( 4.243569643750003451, -22.51708695574430763, -12.14774289770557303 ) ) ;
#11063 = CARTESIAN_POINT ( 'NONE',  ( 0.5181399714639640663, -10.00000000000201794, -3.173488174263044304 ) ) ;
#11064 = EDGE_CURVE ( 'NONE', #5475, #1278, #13235, .T. ) ;
#11065 = CARTESIAN_POINT ( 'NONE',  ( 0.000000000000000000, 5.977523610840987267, 32.81826849749789687 ) ) ;
#11066 = CARTESIAN_POINT ( 'NONE',  ( 0.000000000000000000, -27.20729309053124112, -14.57456132866985499 ) ) ;
#11067 = CARTESIAN_POINT ( 'NONE',  ( -4.243569643749997233, -19.55958345580923918, -7.923990169340445533 ) ) ;
#11068 = EDGE_CURVE ( 'NONE', #10009, #1326, #13780, .T. ) ;
#11069 = LINE ( 'NONE', #2562, #15987 ) ;
#11070 = CARTESIAN_POINT ( 'NONE',  ( 0.8262555684461332373, 37.24680007765648071, 2.360188852285403982 ) ) ;
#11071 = CARTESIAN_POINT ( 'NONE',  ( -1.661723472263481630E-14, -20.05904396871067874, -11.33959077613006450 ) ) ;
#11072 = CARTESIAN_POINT ( 'NONE',  ( 3.500000000000000444, 39.24680007765647360, -0.05647727720536935281 ) ) ;
#11073 = LINE ( 'NONE', #18062, #13692 ) ;
#11074 = CARTESIAN_POINT ( 'NONE',  ( -1.454122949574299328, 15.00000000000144595, -3.397310229520432934 ) ) ;
#11075 = VERTEX_POINT ( 'NONE', #17806 ) ;
#11076 = CARTESIAN_POINT ( 'NONE',  ( -4.243569643750004339, -24.07893542801298281, -5.835313456926535025 ) ) ;
#11077 = CARTESIAN_POINT ( 'NONE',  ( 1.135272562821090458, 22.24680007765648071, 3.311245368580554072 ) ) ;
#11078 = CARTESIAN_POINT ( 'NONE',  ( -5.040478647146445113, -10.97734431112249531, 19.36653379754668336 ) ) ;
#11079 = CARTESIAN_POINT ( 'NONE',  ( -5.330712181944246111E-15, -30.65656652402004312, -10.95765408413266861 ) ) ;
#11080 = DIRECTION ( 'NONE',  ( 0.000000000000000000, 0.000000000000000000, 1.000000000000000000 ) ) ;
#11081 = CARTESIAN_POINT ( 'NONE',  ( -2.000000000000005773, -25.22687694484738685, -5.706757097073694496 ) ) ;
#11082 = EDGE_CURVE ( 'NONE', #3053, #3352, #14399, .T. ) ;
#11083 = CARTESIAN_POINT ( 'NONE',  ( -10.00000000000000000, 43.00000000000000000, 2.499999999999998224 ) ) ;
#11084 = CARTESIAN_POINT ( 'NONE',  ( 4.243569643750000786, -26.32004204090319632, -13.30743551066369257 ) ) ;
#11085 = VERTEX_POINT ( 'NONE', #1004 ) ;
#11086 = CARTESIAN_POINT ( 'NONE',  ( -2.000000000000005773, -26.25931453027926210, -7.181230776793885440 ) ) ;
#11087 = CARTESIAN_POINT ( 'NONE',  ( -5.279047395330986450E-15, -26.21577048483363015, -5.105884481545933440 ) ) ;
#11088 = CARTESIAN_POINT ( 'NONE',  ( 3.481649420246369697, 39.12180007765646650, -1.193696214020541824 ) ) ;
#11089 = ORIENTED_EDGE ( 'NONE', *, *, #5591, .F. ) ;
#11090 =( BOUNDED_SURFACE ( )  B_SPLINE_SURFACE ( 3, 2, ( 
 ( #12530, #9293, #13930, #5307, #10958, #16642, #4007, #7895, #1144, #15057, #3914, #5397, #3820, #1238, #9568, #15245, #5119, #10776, #16545, #2361, #2540, #6782, #12438, #16820, #963, #12162, #18130, #2451, #13552, #12254, #868, #17940, #5213, #3730, #15773, #5840, #14380, #9834, #12978, #7136, #6959, #11583, #10093, #12799, #4188, #9919, #2981, #15592, #9745, #4457, #1417, #3072, #1683, #17005, #15512, #11396, #4276, #14290, #17087, #1328, #106, #14106, #5760, #2892, #15427, #7046, #12709, #8527, #7316, #11224, #2724, #293, #8705, #5935, #5666, #11489, #12617, #14, #4094, #16911, #1501, #4359, #18305, #14198, #11310, #8356, #14017, #17184, #5575, #2808, #10010, #15686, #8438, #8612, #1593, #7227, #12885, #191, #12209, #7413, #6648, #6119, #10381, #10190, #8802, #3260, #15869, #475, #17276, #9336, #7511, #15013, #13601, #14484, #9000, #1878, #915, #4549, #6558, #13072, #9425, #3353, #14675, #17370, #16405, #6026, #1783, #16495, #12117, #17894, #388, #3166, #11769, #16061, #11676, #4635, #8897, #10284, #17465, #15968, #2311, #13164, #7944, #5166, #14575, #1973, #4734, #10820, #7598, #13507, #823, #6467, #3690, #15101, #3773, #17812, #1009, #5073, #10730, #2404, #8036, #13695, #4042, #9694, #15377, #14056, #10914, #16865, #12392, #2676, #8395, #6828, #5623, #6915, #8312, #8127, #2497, #13881, #5351, #13967, #12571, #1283, #2847, #11003, #15196, #11175, #1191, #12475, #16682, #11088, #9612, #15284, #9515, #11267, #1367, #4235, #18080, #8477, #18259, #13785, #1461 ),
 ( #17987, #12660, #2584, #18351, #9876, #18173, #3959, #5529, #5441, #4141, #9789, #1096, #15470, #8217, #2766, #16773, #5258, #6998, #16955, #15551, #14149, #6736, #16590, #12297, #3869, #16012, #8660, #8849, #15637, #4409, #3304, #14244, #4502, #8754, #4315, #1635, #3026, #4683, #17417, #11536, #17229, #7185, #5979, #1547, #9962, #6069, #1732, #1826, #2936, #14626, #14337, #242, #58, #17044, #11441, #5716, #7272, #7091, #17325, #15728, #4589, #3214, #8571, #10145, #10051, #14529, #12757, #15824, #5888, #12843, #11632, #10333, #7462, #147, #8946, #3120, #12928, #11355, #5797, #13122, #14428, #7366, #13026, #431, #17132, #10238, #341, #15915, #11723, #14813, #13573, #14909, #12001, #16109, #10429, #3486, #13309, #4960, #2203, #3577, #10801, #622, #4777, #799, #9133, #2111, #6261, #711, #17610, #4872, #17515, #893, #3671, #12187, #7643, #16470, #10615, #3399, #9401, #7919, #16290, #2016, #7741, #6445, #13399, #7553, #2290, #10522, #6535, #17874, #6359, #11913, #9227, #17695, #12093, #7829, #9042, #13485, #16195, #17789, #5050, #13208, #10706, #16382, #9316, #5143, #14718, #525, #3752, #1929, #6170, #14989, #11819, #5234, #12365, #5604, #3848, #12456, #16753, #12276, #9588, #10983, #12641, #2382, #4121, #10889, #2475, #4027, #15267, #6893, #9674, #17965, #5421, #6714, #11070, #2564, #8014, #18059, #5332, #8196, #18331, #9493, #13667, #11249, #8376, #16937, #16661, #16844, #16568, #3938, #4210, #15171, #18152, #15355, #8105, #13859, #1167, #15078, #987, #9770, #13764 ),
 ( #6631, #1076, #6807, #2654, #8291, #13948, #14038, #1347, #1261, #12552, #18238, #5507, #6979, #11154, #15447, #2743, #1528, #11702, #1711, #4573, #6053, #7070, #14318, #5957, #15533, #9857, #318, #14510, #14128, #8550, #15707, #11517, #1616, #5868, #10122, #1807, #2829, #8458, #3005, #1440, #15895, #8640, #17397, #7345, #7249, #4480, #219, #11612, #8731, #11420, #12908, #12738, #17208, #7442, #12823, #126, #17111, #15803, #3099, #39, #3192, #5693, #13101, #2916, #14225, #4386, #4297, #13006, #11333, #14404, #10031, #17027, #17307, #10216, #9943, #415, #8831, #15614, #7163, #5778, #3564, #9116, #1997, #3287, #6427, #16272, #873, #14794, #15995, #16089, #3650, #17494, #13189, #9023, #696, #10412, #14700, #5035, #7900, #504, #3382, #11798, #4854, #602, #16363, #9297, #13556, #14605, #6519, #11985, #14976, #2273, #12073, #9210, #7624, #12167, #14888, #17772, #4662, #1907, #2092, #782, #10312, #8923, #13471, #7537, #6149, #13290, #10505, #6341, #7720, #17679, #4941, #4760, #6242, #11892, #16175, #17591, #10689, #3471, #13381, #2185, #10597, #7813, #8178, #13935, #16736, #1059, #16647, #16453, #10965, #9750, #2457, #8087, #6694, #3920, #11055, #6965, #11139, #17858, #4100, #10870, #3826, #12348, #12258, #15335, #9384, #2546, #18040, #5123, #2635, #6788, #17944, #2729, #9572, #13838, #1243, #8362, #4013, #15251, #15152, #3734, #6877, #9656, #14022, #1333, #5312, #1148, #8275, #12444, #16550, #12535, #13748, #15432, #18224, #18136, #5493, #5404, #16827, #13650, #10780 ),
 ( #15062, #2365, #6614, #7996, #970, #5216, #9477, #5764, #5583, #4194, #17011, #11230, #14204, #1788, #4462, #2898, #10099, #8712, #9841, #4364, #15597, #14385, #12623, #10015, #11401, #1424, #11494, #10195, #1689, #21, #14489, #15690, #8533, #15875, #18312, #12984, #2988, #8619, #14297, #7322, #16918, #17189, #12715, #1598, #298, #7143, #5940, #7232, #12890, #8442, #2814, #1508, #5672, #197, #5848, #15781, #3171, #11317, #15517, #3079, #12805, #111, #4282, #17093, #9925, #11589, #14112, #17285, #4554, #8808, #7052, #16337, #10484, #10292, #14958, #13449, #16158, #7517, #13264, #6319, #582, #13077, #7794, #4740, #763, #5011, #1977, #13169, #14772, #7603, #17660, #2070, #4640, #3450, #17471, #9091, #6223, #395, #10388, #16066, #11872, #10667, #14581, #6031, #3628, #6408, #9278, #9006, #9186, #15973, #3361, #7420, #1886, #4836, #7699, #3266, #17564, #14681, #11682, #17375, #14867, #8904, #17749, #13360, #672, #482, #11968, #6125, #11776, #12053, #4922, #2162, #10573, #16248, #3542, #3801, #6673, #13815, #9724, #13910, #2253, #6855, #13629, #6585, #9456, #15039, #18110, #12142, #5285, #15129, #7878, #5380, #9545, #2344, #5468, #1033, #10940, #16712, #11113, #1126, #12327, #17922, #852, #3985, #6761, #16802, #4072, #2433, #8059, #12419, #13722, #941, #15312, #5194, #12509, #9634, #16623, #11029, #18013, #10846, #16434, #3898, #2523, #17835, #15223, #6497, #8153, #12236, #2611, #1218, #8251, #18204, #16522, #13535, #5099, #10759, #3713, #9363, #7976, #14364, #9813 ),
 ( #1663, #9989, #10077, #5556, #4531, #4259, #8504, #8336, #6942, #1396, #13995, #16982, #15409, #7212, #5647, #12866, #11469, #12595, #7118, #1568, #17163, #2704, #12778, #14177, #4170, #14271, #12959, #4437, #2791, #17258, #87, #11290, #274, #1310, #15756, #5740, #11380, #17067, #3056, #18283, #1574, #15494, #4342, #8687, #9902, #7299, #15664, #2962, #11204, #16893, #15573, #8422, #8596, #173, #5824, #5918, #1484, #14084, #11563, #7023, #12688, #2874, #12030, #7582, #6101, #7769, #10173, #10548, #1956, #13240, #558, #11947, #8782, #14749, #10267, #6200, #6293, #4715, #3517, #4814, #11849, #6007, #368, #11753, #3244, #17544, #10462, #16140, #743, #8882, #13057, #9070, #17447, #10365, #14560, #8983, #7491, #13149, #7397, #9164, #17641, #2138, #15947, #6387, #3429, #11662, #17723, #16224, #2046, #1860, #16045, #7676, #3337, #15850, #14845, #460, #13429, #3147, #14656, #13340, #650, #4898, #14462, #1766, #17354, #4617, #15018, #1013, #17900, #16317, #7949, #2318, #16500, #8222, #12122, #10645, #2588, #16685, #13886, #6562, #6740, #13513, #13606, #1196, #17816, #2409, #6654, #2230, #5170, #920, #6832, #3602, #12396, #829, #15288, #9431, #15106, #5077, #3874, #10736, #7856, #3963, #17992, #18085, #6470, #12481, #12213, #3779, #9253, #14938, #9340, #16410, #10824, #4989, #15202, #8040, #2501, #1100, #3694, #13701, #12301, #5358, #5264, #10918, #11006, #16596, #8130, #9520, #13790, #9615, #15474, #12665, #16776, #9794, #4047, #14059, #6919, #2771, #14408, #15807, #8734 ),
 ( #13974, #1714, #8314, #9697, #12575, #1371, #1288, #18262, #3103, #13009, #15382, #5532, #2681, #16868, #11180, #7348, #322, #5960, #4147, #18176, #7001, #5445, #11092, #8401, #222, #5870, #11521, #17211, #4483, #10126, #13567, #2468, #12703, #3662, #16375, #7039, #2887, #2282, #15071, #3839, #18051, #8096, #12359, #16655, #8520, #9308, #14982, #9486, #7912, #4271, #15162, #99, #8433, #13758, #10977, #6705, #9, #15260, #17955, #1068, #884, #5324, #14193, #980, #6624, #5227, #3931, #9581, #5755, #9914, #6528, #1496, #9394, #2376, #10881, #10791, #14100, #12178, #2556, #16561, #17867, #1411, #5660, #16462, #7131, #11304, #16998, #15587, #12794, #5133, #3743, #13660, #8006, #12268, #4632, #7595, #13253, #289, #17272, #10280, #4544, #10089, #6116, #8701, #3350, #15962, #15864, #14375, #10005, #13161, #3257, #572, #11391, #5931, #10186, #8895, #3161, #15769, #11766, #1679, #8997, #7505, #14478, #14572, #8798, #7312, #7223, #1780, #11673, #2977, #7410, #15682, #13069, #3068, #384, #10378, #471, #17460, #12972, #4730, #11578, #1875, #16057, #17083, #14671, #1589, #1969, #6022, #17367, #11483, #4355, #187, #14286, #8607, #12880, #5836, #17180, #4452, #10676, #1043, #18023, #6330, #5296, #3722, #8073, #6682, #3810, #954, #6417, #16633, #6597, #9466, #10949, #11976, #860, #10857, #2079, #14781, #5205, #12336, #683, #13461, #2263, #16443, #6508, #10768, #15048, #3906, #7709, #13368, #7887, #17668, #2442, #13545, #4931, #12243, #12154, #9373, #5110, #16533, #13639 ),
 ( #10584, #7802, #16260, #17932, #3640, #9286, #771, #17844, #12061, #17759, #3552, #13732, #15138, #9195, #2172, #14876, #2354, #5023, #16346, #14966, #7984, #9643, #15418, #8430, #2621, #12606, #9823, #11213, #96, #8261, #12429, #14094, #16812, #4082, #13920, #8346, #6864, #12520, #6771, #2884, #11300, #1493, #15321, #5750, #18296, #18121, #17079, #15582, #5566, #1229, #2714, #1408, #14006, #15234, #9911, #18212, #8516, #7128, #9735, #5480, #16903, #1318, #7036, #4179, #5389, #15505, #11124, #2800, #6951, #2532, #12698, #6, #5657, #12790, #16723, #8161, #11388, #14189, #9558, #16993, #4268, #11040, #13826, #1135, #3997, #1776, #6019, #1585, #468, #15860, #6111, #11858, #11763, #12875, #14667, #8793, #14475, #4448, #3252, #11480, #7220, #3347, #17363, #17457, #7590, #8604, #10086, #14569, #15677, #14282, #8697, #2974, #5928, #4351, #1871, #12969, #7501, #4724, #182, #7406, #7309, #10375, #10000, #13065, #3157, #17174, #8891, #1965, #16054, #15766, #6210, #380, #284, #13250, #5833, #8993, #11670, #4628, #10277, #569, #3065, #13158, #14372, #15958, #1674, #17269, #11574, #4541, #10183, #13349, #7687, #751, #1023, #14947, #13438, #15113, #17554, #17911, #9263, #2239, #7865, #929, #16147, #3702, #17649, #13523, #13616, #12039, #10834, #12130, #839, #659, #6305, #6396, #10559, #6481, #17824, #5086, #8048, #16236, #2057, #16420, #17735, #4999, #3527, #16327, #14854, #2147, #14759, #16509, #6571, #9441, #4907, #13711, #10747, #11956, #6663, #5179, #9349, #9174, #10655 ) ),
 .UNSPECIFIED., .T., .F., .T. ) 
 B_SPLINE_SURFACE_WITH_KNOTS ( ( 4, 3, 4 ),
 ( 3, 2, 2, 2, 2, 2, 2, 2, 2, 2, 2, 2, 2, 2, 2, 2, 2, 2, 2, 2, 2, 2, 2, 2, 2, 2, 2, 2, 2, 2, 2, 2, 2, 2, 2, 2, 2, 2, 2, 2, 2, 2, 2, 2, 2, 2, 2, 2, 2, 2, 2, 2, 2, 2, 2, 2, 2, 2, 2, 2, 2, 2, 2, 2, 2, 2, 2, 2, 2, 2, 2, 2, 2, 2, 2, 2, 2, 2, 2, 2, 2, 2, 2, 2, 2, 2, 2, 2, 2, 2, 2, 2, 2, 2, 2, 2, 2, 2, 2, 2, 3 ),
 ( 0.000000000000000000, 0.5000000000000000000, 1.000000000000000000 ),
 ( 0.000000000000000000, 0.01000000000000000021, 0.02000000000000000042, 0.02999999999999999889, 0.04000000000000000083, 0.05000000000000000278, 0.05999999999999999778, 0.07000000000000000666, 0.08000000000000000167, 0.08999999999999999667, 0.1000000000000000056, 0.1100000000000000006, 0.1199999999999999956, 0.1300000000000000044, 0.1400000000000000133, 0.1499999999999999944, 0.1600000000000000033, 0.1700000000000000122, 0.1799999999999999933, 0.1900000000000000022, 0.2000000000000000111, 0.2099999999999999922, 0.2200000000000000011, 0.2300000000000000100, 0.2399999999999999911, 0.2500000000000000000, 0.2600000000000000089, 0.2700000000000000178, 0.2800000000000000266, 0.2899999999999999800, 0.2999999999999999889, 0.3099999999999999978, 0.3200000000000000067, 0.3300000000000000155, 0.3400000000000000244, 0.3499999999999999778, 0.3599999999999999867, 0.3699999999999999956, 0.3800000000000000044, 0.3900000000000000133, 0.4000000000000000222, 0.4099999999999999756, 0.4199999999999999845, 0.4299999999999999933, 0.4400000000000000022, 0.4500000000000000111, 0.4600000000000000200, 0.4699999999999999734, 0.4799999999999999822, 0.4899999999999999911, 0.5000000000000000000, 0.5100000000000000089, 0.5200000000000000178, 0.5300000000000000266, 0.5400000000000000355, 0.5500000000000000444, 0.5600000000000000533, 0.5699999999999999512, 0.5799999999999999600, 0.5899999999999999689, 0.5999999999999999778, 0.6099999999999999867, 0.6199999999999999956, 0.6300000000000000044, 0.6400000000000000133, 0.6500000000000000222, 0.6600000000000000311, 0.6700000000000000400, 0.6800000000000000488, 0.6899999999999999467, 0.6999999999999999556, 0.7099999999999999645, 0.7199999999999999734, 0.7299999999999999822, 0.7399999999999999911, 0.7500000000000000000, 0.7600000000000000089, 0.7700000000000000178, 0.7800000000000000266, 0.7900000000000000355, 0.8000000000000000444, 0.8100000000000000533, 0.8199999999999999512, 0.8299999999999999600, 0.8399999999999999689, 0.8499999999999999778, 0.8599999999999999867, 0.8699999999999999956, 0.8800000000000000044, 0.8900000000000000133, 0.9000000000000000222, 0.9100000000000000311, 0.9200000000000000400, 0.9300000000000000488, 0.9399999999999999467, 0.9499999999999999556, 0.9599999999999999645, 0.9699999999999999734, 0.9799999999999999822, 0.9899999999999999911, 1.000000000000000000 ),
 .UNSPECIFIED. ) 
 GEOMETRIC_REPRESENTATION_ITEM ( )  RATIONAL_B_SPLINE_SURFACE ( (
 ( 1.000000000000000000, 0.9510565162951535312, 1.000000000000000000, 0.9510565162951535312, 1.000000000000000000, 0.9510565162951535312, 1.000000000000000000, 0.9510565162951535312, 1.000000000000000000, 0.9510565162951535312, 1.000000000000000000, 0.9510565162951535312, 1.000000000000000000, 0.9510565162951535312, 1.000000000000000000, 0.9510565162951535312, 1.000000000000000000, 0.9510565162951535312, 1.000000000000000000, 0.9510565162951535312, 1.000000000000000000, 0.9510565162951535312, 1.000000000000000000, 0.9510565162951535312, 1.000000000000000000, 0.9510565162951535312, 1.000000000000000000, 0.9510565162951535312, 1.000000000000000000, 0.9510565162951535312, 1.000000000000000000, 0.9510565162951535312, 1.000000000000000000, 0.9510565162951535312, 1.000000000000000000, 0.9510565162951535312, 1.000000000000000000, 0.9510565162951535312, 1.000000000000000000, 0.9510565162951535312, 1.000000000000000000, 0.9510565162951535312, 1.000000000000000000, 0.9510565162951535312, 1.000000000000000000, 0.9510565162951535312, 1.000000000000000000, 0.9510565162951535312, 1.000000000000000000, 0.9510565162951535312, 1.000000000000000000, 0.9510565162951535312, 1.000000000000000000, 0.9510565162951535312, 1.000000000000000000, 0.9510565162951535312, 1.000000000000000000, 0.9510565162951535312, 1.000000000000000000, 0.9510565162951535312, 1.000000000000000000, 0.9510565162951535312, 1.000000000000000000, 0.9510565162951535312, 1.000000000000000000, 0.9510565162951535312, 1.000000000000000000, 0.9510565162951535312, 1.000000000000000000, 0.9510565162951535312, 1.000000000000000000, 0.9510565162951535312, 1.000000000000000000, 0.9510565162951535312, 1.000000000000000000, 0.9510565162951535312, 1.000000000000000000, 0.9510565162951535312, 1.000000000000000000, 0.9510565162951535312, 1.000000000000000000, 0.9510565162951535312, 1.000000000000000000, 0.9510565162951535312, 1.000000000000000000, 0.9510565162951535312, 1.000000000000000000, 0.9510565162951535312, 1.000000000000000000, 0.9510565162951535312, 1.000000000000000000, 0.9510565162951535312, 1.000000000000000000, 0.9510565162951535312, 1.000000000000000000, 0.9510565162951535312, 1.000000000000000000, 0.9510565162951535312, 1.000000000000000000, 0.9510565162951535312, 1.000000000000000000, 0.9510565162951535312, 1.000000000000000000, 0.9510565162951535312, 1.000000000000000000, 0.9510565162951535312, 1.000000000000000000, 0.9510565162951535312, 1.000000000000000000, 0.9510565162951535312, 1.000000000000000000, 0.9510565162951535312, 1.000000000000000000, 0.9510565162951535312, 1.000000000000000000, 0.9510565162951535312, 1.000000000000000000, 0.9510565162951535312, 1.000000000000000000, 0.9510565162951535312, 1.000000000000000000, 0.9510565162951535312, 1.000000000000000000, 0.9510565162951535312, 1.000000000000000000, 0.9510565162951535312, 1.000000000000000000, 0.9510565162951535312, 1.000000000000000000, 0.9510565162951535312, 1.000000000000000000, 0.9510565162951535312, 1.000000000000000000, 0.9510565162951535312, 1.000000000000000000, 0.9510565162951535312, 1.000000000000000000, 0.9510565162951535312, 1.000000000000000000, 0.9510565162951535312, 1.000000000000000000, 0.9510565162951535312, 1.000000000000000000, 0.9510565162951535312, 1.000000000000000000, 0.9510565162951535312, 1.000000000000000000, 0.9510565162951535312, 1.000000000000000000, 0.9510565162951535312, 1.000000000000000000, 0.9510565162951535312, 1.000000000000000000, 0.9510565162951535312, 1.000000000000000000, 0.9510565162951535312, 1.000000000000000000, 0.9510565162951535312, 1.000000000000000000, 0.9510565162951535312, 1.000000000000000000, 0.9510565162951535312, 1.000000000000000000, 0.9510565162951535312, 1.000000000000000000, 0.9510565162951535312, 1.000000000000000000, 0.9510565162951535312, 1.000000000000000000, 0.9510565162951535312, 1.000000000000000000, 0.9510565162951535312, 1.000000000000000000, 0.9510565162951535312, 1.000000000000000000, 0.9510565162951535312, 1.000000000000000000, 0.9510565162951535312, 1.000000000000000000, 0.9510565162951535312, 1.000000000000000000, 0.9510565162951535312, 1.000000000000000000, 0.9510565162951535312, 1.000000000000000000, 0.9510565162951535312, 1.000000000000000000, 0.9510565162951535312, 1.000000000000000000, 0.9510565162951535312, 1.000000000000000000, 0.9510565162951535312, 1.000000000000000000, 0.9510565162951535312, 1.000000000000000000, 0.9510565162951535312, 1.000000000000000000, 0.9510565162951535312, 1.000000000000000000, 0.9510565162951535312, 1.000000000000000000),
 ( 0.3333333333333333703, 0.3170188387650512141, 0.3333333333333333703, 0.3170188387650512141, 0.3333333333333333703, 0.3170188387650512141, 0.3333333333333333703, 0.3170188387650512141, 0.3333333333333333703, 0.3170188387650512141, 0.3333333333333333703, 0.3170188387650512141, 0.3333333333333333703, 0.3170188387650512141, 0.3333333333333333703, 0.3170188387650512141, 0.3333333333333333703, 0.3170188387650512141, 0.3333333333333333703, 0.3170188387650512141, 0.3333333333333333703, 0.3170188387650512141, 0.3333333333333333703, 0.3170188387650512141, 0.3333333333333333703, 0.3170188387650512141, 0.3333333333333333703, 0.3170188387650512141, 0.3333333333333333703, 0.3170188387650512141, 0.3333333333333333703, 0.3170188387650512141, 0.3333333333333333703, 0.3170188387650512141, 0.3333333333333333703, 0.3170188387650512141, 0.3333333333333333703, 0.3170188387650512141, 0.3333333333333333703, 0.3170188387650512141, 0.3333333333333333703, 0.3170188387650512141, 0.3333333333333333703, 0.3170188387650512141, 0.3333333333333333703, 0.3170188387650512141, 0.3333333333333333703, 0.3170188387650512141, 0.3333333333333333703, 0.3170188387650512141, 0.3333333333333333703, 0.3170188387650512141, 0.3333333333333333703, 0.3170188387650512141, 0.3333333333333333703, 0.3170188387650512141, 0.3333333333333333703, 0.3170188387650512141, 0.3333333333333333703, 0.3170188387650512141, 0.3333333333333333703, 0.3170188387650512141, 0.3333333333333333703, 0.3170188387650512141, 0.3333333333333333703, 0.3170188387650512141, 0.3333333333333333703, 0.3170188387650512141, 0.3333333333333333703, 0.3170188387650512141, 0.3333333333333333703, 0.3170188387650512141, 0.3333333333333333703, 0.3170188387650512141, 0.3333333333333333703, 0.3170188387650512141, 0.3333333333333333703, 0.3170188387650512141, 0.3333333333333333703, 0.3170188387650512141, 0.3333333333333333703, 0.3170188387650512141, 0.3333333333333333703, 0.3170188387650512141, 0.3333333333333333703, 0.3170188387650512141, 0.3333333333333333703, 0.3170188387650512141, 0.3333333333333333703, 0.3170188387650512141, 0.3333333333333333703, 0.3170188387650512141, 0.3333333333333333703, 0.3170188387650512141, 0.3333333333333333703, 0.3170188387650512141, 0.3333333333333333703, 0.3170188387650512141, 0.3333333333333333703, 0.3170188387650512141, 0.3333333333333333703, 0.3170188387650512141, 0.3333333333333333703, 0.3170188387650512141, 0.3333333333333333703, 0.3170188387650512141, 0.3333333333333333703, 0.3170188387650512141, 0.3333333333333333703, 0.3170188387650512141, 0.3333333333333333703, 0.3170188387650512141, 0.3333333333333333703, 0.3170188387650512141, 0.3333333333333333703, 0.3170188387650512141, 0.3333333333333333703, 0.3170188387650512141, 0.3333333333333333703, 0.3170188387650512141, 0.3333333333333333703, 0.3170188387650512141, 0.3333333333333333703, 0.3170188387650512141, 0.3333333333333333703, 0.3170188387650512141, 0.3333333333333333703, 0.3170188387650512141, 0.3333333333333333703, 0.3170188387650512141, 0.3333333333333333703, 0.3170188387650512141, 0.3333333333333333703, 0.3170188387650512141, 0.3333333333333333703, 0.3170188387650512141, 0.3333333333333333703, 0.3170188387650512141, 0.3333333333333333703, 0.3170188387650512141, 0.3333333333333333703, 0.3170188387650512141, 0.3333333333333333703, 0.3170188387650512141, 0.3333333333333333703, 0.3170188387650512141, 0.3333333333333333703, 0.3170188387650512141, 0.3333333333333333703, 0.3170188387650512141, 0.3333333333333333703, 0.3170188387650512141, 0.3333333333333333703, 0.3170188387650512141, 0.3333333333333333703, 0.3170188387650512141, 0.3333333333333333703, 0.3170188387650512141, 0.3333333333333333703, 0.3170188387650512141, 0.3333333333333333703, 0.3170188387650512141, 0.3333333333333333703, 0.3170188387650512141, 0.3333333333333333703, 0.3170188387650512141, 0.3333333333333333703, 0.3170188387650512141, 0.3333333333333333703, 0.3170188387650512141, 0.3333333333333333703, 0.3170188387650512141, 0.3333333333333333703, 0.3170188387650512141, 0.3333333333333333703, 0.3170188387650512141, 0.3333333333333333703, 0.3170188387650512141, 0.3333333333333333703, 0.3170188387650512141, 0.3333333333333333703, 0.3170188387650512141, 0.3333333333333333703, 0.3170188387650512141, 0.3333333333333333703, 0.3170188387650512141, 0.3333333333333333703, 0.3170188387650512141, 0.3333333333333333703, 0.3170188387650512141, 0.3333333333333333703, 0.3170188387650512141, 0.3333333333333333703, 0.3170188387650512141, 0.3333333333333333703, 0.3170188387650512141, 0.3333333333333333703, 0.3170188387650512141, 0.3333333333333333703, 0.3170188387650512141, 0.3333333333333333703),
 ( 0.3333333333333333703, 0.3170188387650512141, 0.3333333333333333703, 0.3170188387650512141, 0.3333333333333333703, 0.3170188387650512141, 0.3333333333333333703, 0.3170188387650512141, 0.3333333333333333703, 0.3170188387650512141, 0.3333333333333333703, 0.3170188387650512141, 0.3333333333333333703, 0.3170188387650512141, 0.3333333333333333703, 0.3170188387650512141, 0.3333333333333333703, 0.3170188387650512141, 0.3333333333333333703, 0.3170188387650512141, 0.3333333333333333703, 0.3170188387650512141, 0.3333333333333333703, 0.3170188387650512141, 0.3333333333333333703, 0.3170188387650512141, 0.3333333333333333703, 0.3170188387650512141, 0.3333333333333333703, 0.3170188387650512141, 0.3333333333333333703, 0.3170188387650512141, 0.3333333333333333703, 0.3170188387650512141, 0.3333333333333333703, 0.3170188387650512141, 0.3333333333333333703, 0.3170188387650512141, 0.3333333333333333703, 0.3170188387650512141, 0.3333333333333333703, 0.3170188387650512141, 0.3333333333333333703, 0.3170188387650512141, 0.3333333333333333703, 0.3170188387650512141, 0.3333333333333333703, 0.3170188387650512141, 0.3333333333333333703, 0.3170188387650512141, 0.3333333333333333703, 0.3170188387650512141, 0.3333333333333333703, 0.3170188387650512141, 0.3333333333333333703, 0.3170188387650512141, 0.3333333333333333703, 0.3170188387650512141, 0.3333333333333333703, 0.3170188387650512141, 0.3333333333333333703, 0.3170188387650512141, 0.3333333333333333703, 0.3170188387650512141, 0.3333333333333333703, 0.3170188387650512141, 0.3333333333333333703, 0.3170188387650512141, 0.3333333333333333703, 0.3170188387650512141, 0.3333333333333333703, 0.3170188387650512141, 0.3333333333333333703, 0.3170188387650512141, 0.3333333333333333703, 0.3170188387650512141, 0.3333333333333333703, 0.3170188387650512141, 0.3333333333333333703, 0.3170188387650512141, 0.3333333333333333703, 0.3170188387650512141, 0.3333333333333333703, 0.3170188387650512141, 0.3333333333333333703, 0.3170188387650512141, 0.3333333333333333703, 0.3170188387650512141, 0.3333333333333333703, 0.3170188387650512141, 0.3333333333333333703, 0.3170188387650512141, 0.3333333333333333703, 0.3170188387650512141, 0.3333333333333333703, 0.3170188387650512141, 0.3333333333333333703, 0.3170188387650512141, 0.3333333333333333703, 0.3170188387650512141, 0.3333333333333333703, 0.3170188387650512141, 0.3333333333333333703, 0.3170188387650512141, 0.3333333333333333703, 0.3170188387650512141, 0.3333333333333333703, 0.3170188387650512141, 0.3333333333333333703, 0.3170188387650512141, 0.3333333333333333703, 0.3170188387650512141, 0.3333333333333333703, 0.3170188387650512141, 0.3333333333333333703, 0.3170188387650512141, 0.3333333333333333703, 0.3170188387650512141, 0.3333333333333333703, 0.3170188387650512141, 0.3333333333333333703, 0.3170188387650512141, 0.3333333333333333703, 0.3170188387650512141, 0.3333333333333333703, 0.3170188387650512141, 0.3333333333333333703, 0.3170188387650512141, 0.3333333333333333703, 0.3170188387650512141, 0.3333333333333333703, 0.3170188387650512141, 0.3333333333333333703, 0.3170188387650512141, 0.3333333333333333703, 0.3170188387650512141, 0.3333333333333333703, 0.3170188387650512141, 0.3333333333333333703, 0.3170188387650512141, 0.3333333333333333703, 0.3170188387650512141, 0.3333333333333333703, 0.3170188387650512141, 0.3333333333333333703, 0.3170188387650512141, 0.3333333333333333703, 0.3170188387650512141, 0.3333333333333333703, 0.3170188387650512141, 0.3333333333333333703, 0.3170188387650512141, 0.3333333333333333703, 0.3170188387650512141, 0.3333333333333333703, 0.3170188387650512141, 0.3333333333333333703, 0.3170188387650512141, 0.3333333333333333703, 0.3170188387650512141, 0.3333333333333333703, 0.3170188387650512141, 0.3333333333333333703, 0.3170188387650512141, 0.3333333333333333703, 0.3170188387650512141, 0.3333333333333333703, 0.3170188387650512141, 0.3333333333333333703, 0.3170188387650512141, 0.3333333333333333703, 0.3170188387650512141, 0.3333333333333333703, 0.3170188387650512141, 0.3333333333333333703, 0.3170188387650512141, 0.3333333333333333703, 0.3170188387650512141, 0.3333333333333333703, 0.3170188387650512141, 0.3333333333333333703, 0.3170188387650512141, 0.3333333333333333703, 0.3170188387650512141, 0.3333333333333333703, 0.3170188387650512141, 0.3333333333333333703, 0.3170188387650512141, 0.3333333333333333703, 0.3170188387650512141, 0.3333333333333333703, 0.3170188387650512141, 0.3333333333333333703, 0.3170188387650512141, 0.3333333333333333703, 0.3170188387650512141, 0.3333333333333333703, 0.3170188387650512141, 0.3333333333333333703, 0.3170188387650512141, 0.3333333333333333703),
 ( 1.000000000000000000, 0.9510565162951535312, 1.000000000000000000, 0.9510565162951535312, 1.000000000000000000, 0.9510565162951535312, 1.000000000000000000, 0.9510565162951535312, 1.000000000000000000, 0.9510565162951535312, 1.000000000000000000, 0.9510565162951535312, 1.000000000000000000, 0.9510565162951535312, 1.000000000000000000, 0.9510565162951535312, 1.000000000000000000, 0.9510565162951535312, 1.000000000000000000, 0.9510565162951535312, 1.000000000000000000, 0.9510565162951535312, 1.000000000000000000, 0.9510565162951535312, 1.000000000000000000, 0.9510565162951535312, 1.000000000000000000, 0.9510565162951535312, 1.000000000000000000, 0.9510565162951535312, 1.000000000000000000, 0.9510565162951535312, 1.000000000000000000, 0.9510565162951535312, 1.000000000000000000, 0.9510565162951535312, 1.000000000000000000, 0.9510565162951535312, 1.000000000000000000, 0.9510565162951535312, 1.000000000000000000, 0.9510565162951535312, 1.000000000000000000, 0.9510565162951535312, 1.000000000000000000, 0.9510565162951535312, 1.000000000000000000, 0.9510565162951535312, 1.000000000000000000, 0.9510565162951535312, 1.000000000000000000, 0.9510565162951535312, 1.000000000000000000, 0.9510565162951535312, 1.000000000000000000, 0.9510565162951535312, 1.000000000000000000, 0.9510565162951535312, 1.000000000000000000, 0.9510565162951535312, 1.000000000000000000, 0.9510565162951535312, 1.000000000000000000, 0.9510565162951535312, 1.000000000000000000, 0.9510565162951535312, 1.000000000000000000, 0.9510565162951535312, 1.000000000000000000, 0.9510565162951535312, 1.000000000000000000, 0.9510565162951535312, 1.000000000000000000, 0.9510565162951535312, 1.000000000000000000, 0.9510565162951535312, 1.000000000000000000, 0.9510565162951535312, 1.000000000000000000, 0.9510565162951535312, 1.000000000000000000, 0.9510565162951535312, 1.000000000000000000, 0.9510565162951535312, 1.000000000000000000, 0.9510565162951535312, 1.000000000000000000, 0.9510565162951535312, 1.000000000000000000, 0.9510565162951535312, 1.000000000000000000, 0.9510565162951535312, 1.000000000000000000, 0.9510565162951535312, 1.000000000000000000, 0.9510565162951535312, 1.000000000000000000, 0.9510565162951535312, 1.000000000000000000, 0.9510565162951535312, 1.000000000000000000, 0.9510565162951535312, 1.000000000000000000, 0.9510565162951535312, 1.000000000000000000, 0.9510565162951535312, 1.000000000000000000, 0.9510565162951535312, 1.000000000000000000, 0.9510565162951535312, 1.000000000000000000, 0.9510565162951535312, 1.000000000000000000, 0.9510565162951535312, 1.000000000000000000, 0.9510565162951535312, 1.000000000000000000, 0.9510565162951535312, 1.000000000000000000, 0.9510565162951535312, 1.000000000000000000, 0.9510565162951535312, 1.000000000000000000, 0.9510565162951535312, 1.000000000000000000, 0.9510565162951535312, 1.000000000000000000, 0.9510565162951535312, 1.000000000000000000, 0.9510565162951535312, 1.000000000000000000, 0.9510565162951535312, 1.000000000000000000, 0.9510565162951535312, 1.000000000000000000, 0.9510565162951535312, 1.000000000000000000, 0.9510565162951535312, 1.000000000000000000, 0.9510565162951535312, 1.000000000000000000, 0.9510565162951535312, 1.000000000000000000, 0.9510565162951535312, 1.000000000000000000, 0.9510565162951535312, 1.000000000000000000, 0.9510565162951535312, 1.000000000000000000, 0.9510565162951535312, 1.000000000000000000, 0.9510565162951535312, 1.000000000000000000, 0.9510565162951535312, 1.000000000000000000, 0.9510565162951535312, 1.000000000000000000, 0.9510565162951535312, 1.000000000000000000, 0.9510565162951535312, 1.000000000000000000, 0.9510565162951535312, 1.000000000000000000, 0.9510565162951535312, 1.000000000000000000, 0.9510565162951535312, 1.000000000000000000, 0.9510565162951535312, 1.000000000000000000, 0.9510565162951535312, 1.000000000000000000, 0.9510565162951535312, 1.000000000000000000, 0.9510565162951535312, 1.000000000000000000, 0.9510565162951535312, 1.000000000000000000, 0.9510565162951535312, 1.000000000000000000, 0.9510565162951535312, 1.000000000000000000, 0.9510565162951535312, 1.000000000000000000, 0.9510565162951535312, 1.000000000000000000, 0.9510565162951535312, 1.000000000000000000, 0.9510565162951535312, 1.000000000000000000, 0.9510565162951535312, 1.000000000000000000, 0.9510565162951535312, 1.000000000000000000, 0.9510565162951535312, 1.000000000000000000, 0.9510565162951535312, 1.000000000000000000, 0.9510565162951535312, 1.000000000000000000, 0.9510565162951535312, 1.000000000000000000),
 ( 0.3333333333333333703, 0.3170188387650512141, 0.3333333333333333703, 0.3170188387650512141, 0.3333333333333333703, 0.3170188387650512141, 0.3333333333333333703, 0.3170188387650512141, 0.3333333333333333703, 0.3170188387650512141, 0.3333333333333333703, 0.3170188387650512141, 0.3333333333333333703, 0.3170188387650512141, 0.3333333333333333703, 0.3170188387650512141, 0.3333333333333333703, 0.3170188387650512141, 0.3333333333333333703, 0.3170188387650512141, 0.3333333333333333703, 0.3170188387650512141, 0.3333333333333333703, 0.3170188387650512141, 0.3333333333333333703, 0.3170188387650512141, 0.3333333333333333703, 0.3170188387650512141, 0.3333333333333333703, 0.3170188387650512141, 0.3333333333333333703, 0.3170188387650512141, 0.3333333333333333703, 0.3170188387650512141, 0.3333333333333333703, 0.3170188387650512141, 0.3333333333333333703, 0.3170188387650512141, 0.3333333333333333703, 0.3170188387650512141, 0.3333333333333333703, 0.3170188387650512141, 0.3333333333333333703, 0.3170188387650512141, 0.3333333333333333703, 0.3170188387650512141, 0.3333333333333333703, 0.3170188387650512141, 0.3333333333333333703, 0.3170188387650512141, 0.3333333333333333703, 0.3170188387650512141, 0.3333333333333333703, 0.3170188387650512141, 0.3333333333333333703, 0.3170188387650512141, 0.3333333333333333703, 0.3170188387650512141, 0.3333333333333333703, 0.3170188387650512141, 0.3333333333333333703, 0.3170188387650512141, 0.3333333333333333703, 0.3170188387650512141, 0.3333333333333333703, 0.3170188387650512141, 0.3333333333333333703, 0.3170188387650512141, 0.3333333333333333703, 0.3170188387650512141, 0.3333333333333333703, 0.3170188387650512141, 0.3333333333333333703, 0.3170188387650512141, 0.3333333333333333703, 0.3170188387650512141, 0.3333333333333333703, 0.3170188387650512141, 0.3333333333333333703, 0.3170188387650512141, 0.3333333333333333703, 0.3170188387650512141, 0.3333333333333333703, 0.3170188387650512141, 0.3333333333333333703, 0.3170188387650512141, 0.3333333333333333703, 0.3170188387650512141, 0.3333333333333333703, 0.3170188387650512141, 0.3333333333333333703, 0.3170188387650512141, 0.3333333333333333703, 0.3170188387650512141, 0.3333333333333333703, 0.3170188387650512141, 0.3333333333333333703, 0.3170188387650512141, 0.3333333333333333703, 0.3170188387650512141, 0.3333333333333333703, 0.3170188387650512141, 0.3333333333333333703, 0.3170188387650512141, 0.3333333333333333703, 0.3170188387650512141, 0.3333333333333333703, 0.3170188387650512141, 0.3333333333333333703, 0.3170188387650512141, 0.3333333333333333703, 0.3170188387650512141, 0.3333333333333333703, 0.3170188387650512141, 0.3333333333333333703, 0.3170188387650512141, 0.3333333333333333703, 0.3170188387650512141, 0.3333333333333333703, 0.3170188387650512141, 0.3333333333333333703, 0.3170188387650512141, 0.3333333333333333703, 0.3170188387650512141, 0.3333333333333333703, 0.3170188387650512141, 0.3333333333333333703, 0.3170188387650512141, 0.3333333333333333703, 0.3170188387650512141, 0.3333333333333333703, 0.3170188387650512141, 0.3333333333333333703, 0.3170188387650512141, 0.3333333333333333703, 0.3170188387650512141, 0.3333333333333333703, 0.3170188387650512141, 0.3333333333333333703, 0.3170188387650512141, 0.3333333333333333703, 0.3170188387650512141, 0.3333333333333333703, 0.3170188387650512141, 0.3333333333333333703, 0.3170188387650512141, 0.3333333333333333703, 0.3170188387650512141, 0.3333333333333333703, 0.3170188387650512141, 0.3333333333333333703, 0.3170188387650512141, 0.3333333333333333703, 0.3170188387650512141, 0.3333333333333333703, 0.3170188387650512141, 0.3333333333333333703, 0.3170188387650512141, 0.3333333333333333703, 0.3170188387650512141, 0.3333333333333333703, 0.3170188387650512141, 0.3333333333333333703, 0.3170188387650512141, 0.3333333333333333703, 0.3170188387650512141, 0.3333333333333333703, 0.3170188387650512141, 0.3333333333333333703, 0.3170188387650512141, 0.3333333333333333703, 0.3170188387650512141, 0.3333333333333333703, 0.3170188387650512141, 0.3333333333333333703, 0.3170188387650512141, 0.3333333333333333703, 0.3170188387650512141, 0.3333333333333333703, 0.3170188387650512141, 0.3333333333333333703, 0.3170188387650512141, 0.3333333333333333703, 0.3170188387650512141, 0.3333333333333333703, 0.3170188387650512141, 0.3333333333333333703, 0.3170188387650512141, 0.3333333333333333703, 0.3170188387650512141, 0.3333333333333333703, 0.3170188387650512141, 0.3333333333333333703, 0.3170188387650512141, 0.3333333333333333703, 0.3170188387650512141, 0.3333333333333333703, 0.3170188387650512141, 0.3333333333333333703, 0.3170188387650512141, 0.3333333333333333703),
 ( 0.3333333333333333703, 0.3170188387650512141, 0.3333333333333333703, 0.3170188387650512141, 0.3333333333333333703, 0.3170188387650512141, 0.3333333333333333703, 0.3170188387650512141, 0.3333333333333333703, 0.3170188387650512141, 0.3333333333333333703, 0.3170188387650512141, 0.3333333333333333703, 0.3170188387650512141, 0.3333333333333333703, 0.3170188387650512141, 0.3333333333333333703, 0.3170188387650512141, 0.3333333333333333703, 0.3170188387650512141, 0.3333333333333333703, 0.3170188387650512141, 0.3333333333333333703, 0.3170188387650512141, 0.3333333333333333703, 0.3170188387650512141, 0.3333333333333333703, 0.3170188387650512141, 0.3333333333333333703, 0.3170188387650512141, 0.3333333333333333703, 0.3170188387650512141, 0.3333333333333333703, 0.3170188387650512141, 0.3333333333333333703, 0.3170188387650512141, 0.3333333333333333703, 0.3170188387650512141, 0.3333333333333333703, 0.3170188387650512141, 0.3333333333333333703, 0.3170188387650512141, 0.3333333333333333703, 0.3170188387650512141, 0.3333333333333333703, 0.3170188387650512141, 0.3333333333333333703, 0.3170188387650512141, 0.3333333333333333703, 0.3170188387650512141, 0.3333333333333333703, 0.3170188387650512141, 0.3333333333333333703, 0.3170188387650512141, 0.3333333333333333703, 0.3170188387650512141, 0.3333333333333333703, 0.3170188387650512141, 0.3333333333333333703, 0.3170188387650512141, 0.3333333333333333703, 0.3170188387650512141, 0.3333333333333333703, 0.3170188387650512141, 0.3333333333333333703, 0.3170188387650512141, 0.3333333333333333703, 0.3170188387650512141, 0.3333333333333333703, 0.3170188387650512141, 0.3333333333333333703, 0.3170188387650512141, 0.3333333333333333703, 0.3170188387650512141, 0.3333333333333333703, 0.3170188387650512141, 0.3333333333333333703, 0.3170188387650512141, 0.3333333333333333703, 0.3170188387650512141, 0.3333333333333333703, 0.3170188387650512141, 0.3333333333333333703, 0.3170188387650512141, 0.3333333333333333703, 0.3170188387650512141, 0.3333333333333333703, 0.3170188387650512141, 0.3333333333333333703, 0.3170188387650512141, 0.3333333333333333703, 0.3170188387650512141, 0.3333333333333333703, 0.3170188387650512141, 0.3333333333333333703, 0.3170188387650512141, 0.3333333333333333703, 0.3170188387650512141, 0.3333333333333333703, 0.3170188387650512141, 0.3333333333333333703, 0.3170188387650512141, 0.3333333333333333703, 0.3170188387650512141, 0.3333333333333333703, 0.3170188387650512141, 0.3333333333333333703, 0.3170188387650512141, 0.3333333333333333703, 0.3170188387650512141, 0.3333333333333333703, 0.3170188387650512141, 0.3333333333333333703, 0.3170188387650512141, 0.3333333333333333703, 0.3170188387650512141, 0.3333333333333333703, 0.3170188387650512141, 0.3333333333333333703, 0.3170188387650512141, 0.3333333333333333703, 0.3170188387650512141, 0.3333333333333333703, 0.3170188387650512141, 0.3333333333333333703, 0.3170188387650512141, 0.3333333333333333703, 0.3170188387650512141, 0.3333333333333333703, 0.3170188387650512141, 0.3333333333333333703, 0.3170188387650512141, 0.3333333333333333703, 0.3170188387650512141, 0.3333333333333333703, 0.3170188387650512141, 0.3333333333333333703, 0.3170188387650512141, 0.3333333333333333703, 0.3170188387650512141, 0.3333333333333333703, 0.3170188387650512141, 0.3333333333333333703, 0.3170188387650512141, 0.3333333333333333703, 0.3170188387650512141, 0.3333333333333333703, 0.3170188387650512141, 0.3333333333333333703, 0.3170188387650512141, 0.3333333333333333703, 0.3170188387650512141, 0.3333333333333333703, 0.3170188387650512141, 0.3333333333333333703, 0.3170188387650512141, 0.3333333333333333703, 0.3170188387650512141, 0.3333333333333333703, 0.3170188387650512141, 0.3333333333333333703, 0.3170188387650512141, 0.3333333333333333703, 0.3170188387650512141, 0.3333333333333333703, 0.3170188387650512141, 0.3333333333333333703, 0.3170188387650512141, 0.3333333333333333703, 0.3170188387650512141, 0.3333333333333333703, 0.3170188387650512141, 0.3333333333333333703, 0.3170188387650512141, 0.3333333333333333703, 0.3170188387650512141, 0.3333333333333333703, 0.3170188387650512141, 0.3333333333333333703, 0.3170188387650512141, 0.3333333333333333703, 0.3170188387650512141, 0.3333333333333333703, 0.3170188387650512141, 0.3333333333333333703, 0.3170188387650512141, 0.3333333333333333703, 0.3170188387650512141, 0.3333333333333333703, 0.3170188387650512141, 0.3333333333333333703, 0.3170188387650512141, 0.3333333333333333703, 0.3170188387650512141, 0.3333333333333333703, 0.3170188387650512141, 0.3333333333333333703, 0.3170188387650512141, 0.3333333333333333703, 0.3170188387650512141, 0.3333333333333333703),
 ( 1.000000000000000000, 0.9510565162951535312, 1.000000000000000000, 0.9510565162951535312, 1.000000000000000000, 0.9510565162951535312, 1.000000000000000000, 0.9510565162951535312, 1.000000000000000000, 0.9510565162951535312, 1.000000000000000000, 0.9510565162951535312, 1.000000000000000000, 0.9510565162951535312, 1.000000000000000000, 0.9510565162951535312, 1.000000000000000000, 0.9510565162951535312, 1.000000000000000000, 0.9510565162951535312, 1.000000000000000000, 0.9510565162951535312, 1.000000000000000000, 0.9510565162951535312, 1.000000000000000000, 0.9510565162951535312, 1.000000000000000000, 0.9510565162951535312, 1.000000000000000000, 0.9510565162951535312, 1.000000000000000000, 0.9510565162951535312, 1.000000000000000000, 0.9510565162951535312, 1.000000000000000000, 0.9510565162951535312, 1.000000000000000000, 0.9510565162951535312, 1.000000000000000000, 0.9510565162951535312, 1.000000000000000000, 0.9510565162951535312, 1.000000000000000000, 0.9510565162951535312, 1.000000000000000000, 0.9510565162951535312, 1.000000000000000000, 0.9510565162951535312, 1.000000000000000000, 0.9510565162951535312, 1.000000000000000000, 0.9510565162951535312, 1.000000000000000000, 0.9510565162951535312, 1.000000000000000000, 0.9510565162951535312, 1.000000000000000000, 0.9510565162951535312, 1.000000000000000000, 0.9510565162951535312, 1.000000000000000000, 0.9510565162951535312, 1.000000000000000000, 0.9510565162951535312, 1.000000000000000000, 0.9510565162951535312, 1.000000000000000000, 0.9510565162951535312, 1.000000000000000000, 0.9510565162951535312, 1.000000000000000000, 0.9510565162951535312, 1.000000000000000000, 0.9510565162951535312, 1.000000000000000000, 0.9510565162951535312, 1.000000000000000000, 0.9510565162951535312, 1.000000000000000000, 0.9510565162951535312, 1.000000000000000000, 0.9510565162951535312, 1.000000000000000000, 0.9510565162951535312, 1.000000000000000000, 0.9510565162951535312, 1.000000000000000000, 0.9510565162951535312, 1.000000000000000000, 0.9510565162951535312, 1.000000000000000000, 0.9510565162951535312, 1.000000000000000000, 0.9510565162951535312, 1.000000000000000000, 0.9510565162951535312, 1.000000000000000000, 0.9510565162951535312, 1.000000000000000000, 0.9510565162951535312, 1.000000000000000000, 0.9510565162951535312, 1.000000000000000000, 0.9510565162951535312, 1.000000000000000000, 0.9510565162951535312, 1.000000000000000000, 0.9510565162951535312, 1.000000000000000000, 0.9510565162951535312, 1.000000000000000000, 0.9510565162951535312, 1.000000000000000000, 0.9510565162951535312, 1.000000000000000000, 0.9510565162951535312, 1.000000000000000000, 0.9510565162951535312, 1.000000000000000000, 0.9510565162951535312, 1.000000000000000000, 0.9510565162951535312, 1.000000000000000000, 0.9510565162951535312, 1.000000000000000000, 0.9510565162951535312, 1.000000000000000000, 0.9510565162951535312, 1.000000000000000000, 0.9510565162951535312, 1.000000000000000000, 0.9510565162951535312, 1.000000000000000000, 0.9510565162951535312, 1.000000000000000000, 0.9510565162951535312, 1.000000000000000000, 0.9510565162951535312, 1.000000000000000000, 0.9510565162951535312, 1.000000000000000000, 0.9510565162951535312, 1.000000000000000000, 0.9510565162951535312, 1.000000000000000000, 0.9510565162951535312, 1.000000000000000000, 0.9510565162951535312, 1.000000000000000000, 0.9510565162951535312, 1.000000000000000000, 0.9510565162951535312, 1.000000000000000000, 0.9510565162951535312, 1.000000000000000000, 0.9510565162951535312, 1.000000000000000000, 0.9510565162951535312, 1.000000000000000000, 0.9510565162951535312, 1.000000000000000000, 0.9510565162951535312, 1.000000000000000000, 0.9510565162951535312, 1.000000000000000000, 0.9510565162951535312, 1.000000000000000000, 0.9510565162951535312, 1.000000000000000000, 0.9510565162951535312, 1.000000000000000000, 0.9510565162951535312, 1.000000000000000000, 0.9510565162951535312, 1.000000000000000000, 0.9510565162951535312, 1.000000000000000000, 0.9510565162951535312, 1.000000000000000000, 0.9510565162951535312, 1.000000000000000000, 0.9510565162951535312, 1.000000000000000000, 0.9510565162951535312, 1.000000000000000000, 0.9510565162951535312, 1.000000000000000000, 0.9510565162951535312, 1.000000000000000000, 0.9510565162951535312, 1.000000000000000000, 0.9510565162951535312, 1.000000000000000000, 0.9510565162951535312, 1.000000000000000000, 0.9510565162951535312, 1.000000000000000000, 0.9510565162951535312, 1.000000000000000000, 0.9510565162951535312, 1.000000000000000000) ) ) 
 REPRESENTATION_ITEM ( '' )  SURFACE ( )  );
#11091 = CARTESIAN_POINT ( 'NONE',  ( 4.299564228933482956E-15, -17.92964144805248594, -8.298488810700408891 ) ) ;
#11092 = CARTESIAN_POINT ( 'NONE',  ( -3.673772985318219053, 18.24680007765647716, -2.599342558260952174 ) ) ;
#11093 = CARTESIAN_POINT ( 'NONE',  ( 4.299564228933482956E-15, -17.15531325897858039, -7.192633550910265683 ) ) ;
#11094 = CARTESIAN_POINT ( 'NONE',  ( 2.518350579753611207, 28.12819992234355126, -0.7558219633769606149 ) ) ;
#11095 = ORIENTED_EDGE ( 'NONE', *, *, #3781, .F. ) ;
#11096 = CARTESIAN_POINT ( 'NONE',  ( -5.330712181944246111E-15, -29.65639261313291186, -9.529257706903733194 ) ) ;
#11097 = CARTESIAN_POINT ( 'NONE',  ( 0.05938372350929014415, 27.37180007765647716, 4.731580009072201776 ) ) ;
#11098 = CARTESIAN_POINT ( 'NONE',  ( -4.000000000000004441, -23.01196377286574091, -4.556692218940495032 ) ) ;
#11099 = ORIENTED_EDGE ( 'NONE', *, *, #16832, .F. ) ;
#11100 = CARTESIAN_POINT ( 'NONE',  ( 4.000000000000000000, 3.518949890710770134, -4.119968255444916849E-15 ) ) ;
#11101 = CARTESIAN_POINT ( 'NONE',  ( 1.300000000000000044, -1.443375672974064328, 2.168404344971008868E-16 ) ) ;
#11102 = DIRECTION ( 'NONE',  ( -0.000000000000000000, -0.5735764363510414965, -0.8191520442889950182 ) ) ;
#11103 = DIRECTION ( 'NONE',  ( 0.000000000000000000, 0.000000000000000000, -1.000000000000000000 ) ) ;
#11104 = CARTESIAN_POINT ( 'NONE',  ( 4.243569643750003451, -21.22653997395446623, -10.30465079805533435 ) ) ;
#11105 = ORIENTED_EDGE ( 'NONE', *, *, #9998, .F. ) ;
#11106 = DIRECTION ( 'NONE',  ( -0.000000000000000000, 1.000000000000000000, -0.000000000000000000 ) ) ;
#11107 = ORIENTED_EDGE ( 'NONE', *, *, #6017, .T. ) ;
#11108 = CARTESIAN_POINT ( 'NONE',  ( -5.279047395330986450E-15, -27.76442686298143769, -7.317595001126219856 ) ) ;
#11109 = DIRECTION ( 'NONE',  ( -1.000000000000000000, -0.000000000000000000, -0.000000000000000000 ) ) ;
#11110 = DIRECTION ( 'NONE',  ( -1.000000000000000000, 0.000000000000000000, 4.336808689942021680E-16 ) ) ;
#11111 = FILL_AREA_STYLE ('',( #12507 ) ) ;
#11112 = ORIENTED_EDGE ( 'NONE', *, *, #12728, .F. ) ;
#11113 = CARTESIAN_POINT ( 'NONE',  ( -2.864755990943222308, 34.25319992234354771, 2.011557305968548093 ) ) ;
#11114 = CARTESIAN_POINT ( 'NONE',  ( -3.481649420246394566, 17.12819992234353705, -1.193696214020467883 ) ) ;
#11115 = CARTESIAN_POINT ( 'NONE',  ( -4.000000000000000888, -26.11032815671481444, -13.00793304497391567 ) ) ;
#11116 = CARTESIAN_POINT ( 'NONE',  ( 2.500000000000001332, 29.24680007765648071, -0.05647727720535888202 ) ) ;
#11117 = EDGE_CURVE ( 'NONE', #13534, #3470, #1425, .T. ) ;
#11118 = CARTESIAN_POINT ( 'NONE',  ( -4.499999999999999112, 22.00319992234354061, -0.05647727720528529505 ) ) ;
#11119 = EDGE_CURVE ( 'NONE', #10036, #6155, #17762, .T. ) ;
#11120 = CARTESIAN_POINT ( 'NONE',  ( -5.279047395330986450E-15, -28.47422770226091160, -8.331295654927085792 ) ) ;
#11121 = ORIENTED_EDGE ( 'NONE', *, *, #10973, .T. ) ;
#11122 = EDGE_CURVE ( 'NONE', #1667, #15966, #13583, .T. ) ;
#11123 = CARTESIAN_POINT ( 'NONE',  ( 2.121784821875004390, -17.36235556323629936, -6.921768590024867329 ) ) ;
#11124 = CARTESIAN_POINT ( 'NONE',  ( 1.027846397803542144, 23.74680007765647716, -3.346150245485522312 ) ) ;
#11125 = CIRCLE ( 'NONE', #8746, 4.000000000000001776 ) ;
#11126 = CARTESIAN_POINT ( 'NONE',  ( -9.000000000000003553, 40.79999999999999716, -2.500000000000001776 ) ) ;
#11127 = EDGE_CURVE ( 'NONE', #15647, #5839, #9683, .T. ) ;
#11128 = CARTESIAN_POINT ( 'NONE',  ( -4.243569643750004339, -24.30478114982620497, -6.157854574365327238 ) ) ;
#11129 = AXIS2_PLACEMENT_3D ( 'NONE', #9216, #9120, #3389 ) ;
#11130 = CARTESIAN_POINT ( 'NONE',  ( 4.000000000000000000, -3.518949890710769246, 4.119968255444916849E-15 ) ) ;
#11131 = CARTESIAN_POINT ( 'NONE',  ( 12.00000000000000178, 48.00000000000000000, 15.00000000000000000 ) ) ;
#11132 = ORIENTED_EDGE ( 'NONE', *, *, #7254, .F. ) ;
#11133 = ORIENTED_EDGE ( 'NONE', *, *, #4387, .T. ) ;
#11134 = CARTESIAN_POINT ( 'NONE',  ( 9.000000000000001776, 31.99999999999999289, -2.500000000000002665 ) ) ;
#11135 = EDGE_CURVE ( 'NONE', #13443, #10810, #14300, .T. ) ;
#11136 = CARTESIAN_POINT ( 'NONE',  ( 9.000000000000001776, 29.79999999999999716, -2.500000000000002665 ) ) ;
#11137 = CARTESIAN_POINT ( 'NONE',  ( -6.938893903907228378E-15, 6.938893903907228378E-15, 30.00000000000000000 ) ) ;
#11138 = ORIENTED_EDGE ( 'NONE', *, *, #4215, .T. ) ;
#11139 = CARTESIAN_POINT ( 'NONE',  ( -2.055738996568281518, 34.25319992234354061, 1.423772053676066962 ) ) ;
#11140 = CARTESIAN_POINT ( 'NONE',  ( 4.243569643750000786, -24.51327626639741553, -10.72710657115335842 ) ) ;
#11141 = CARTESIAN_POINT ( 'NONE',  ( -2.211161402132902243, 30.87180007765647716, -2.942372952327172886 ) ) ;
#11142 = CARTESIAN_POINT ( 'NONE',  ( 1.135272562821020070, 30.25319992234354416, -3.311245368580577164 ) ) ;
#11143 = DIRECTION ( 'NONE',  ( -0.000000000000000000, -1.000000000000000000, -0.000000000000000000 ) ) ;
#11144 = AXIS2_PLACEMENT_3D ( 'NONE', #14330, #3114, #11530 ) ;
#11145 = DIRECTION ( 'NONE',  ( -3.469446951953613696E-16, -0.000000000000000000, -1.000000000000000000 ) ) ;
#11146 = CARTESIAN_POINT ( 'NONE',  ( -2.121784821874996396, -20.41665008680558913, -11.28375322586376939 ) ) ;
#11147 = DIRECTION ( 'NONE',  ( -3.373073425510457965E-16, 0.000000000000000000, -1.000000000000000000 ) ) ;
#11148 = LINE ( 'NONE', #13943, #13318 ) ;
#11149 = CARTESIAN_POINT ( 'NONE',  ( -9.184850993605147944E-16, 43.00000000000000000, -10.50000000000000000 ) ) ;
#11150 = CIRCLE ( 'NONE', #16502, 10.00000000000000178 ) ;
#11151 = CARTESIAN_POINT ( 'NONE',  ( 2.121784821875004390, -19.13685766319732906, -9.456020227043945070 ) ) ;
#11152 = FACE_BOUND ( 'NONE', #8100, .T. ) ;
#11153 = PRESENTATION_STYLE_ASSIGNMENT (( #37 ) ) ;
#11154 = CARTESIAN_POINT ( 'NONE',  ( 1.497042530366522461, 16.12819992234354416, 2.161531897785029965 ) ) ;
#11155 = CARTESIAN_POINT ( 'NONE',  ( -9.000000000000001776, 27.59999999999999432, 2.499999999999995559 ) ) ;
#11156 = CARTESIAN_POINT ( 'NONE',  ( -2.864755990943265829, 35.74680007765648071, -2.011557305968488141 ) ) ;
#11157 = CARTESIAN_POINT ( 'NONE',  ( 4.000000000000000888, -25.72316406217786522, -12.45500541507884051 ) ) ;
#11158 = CARTESIAN_POINT ( 'NONE',  ( -11.99999999999999822, 13.00000000000000178, -15.00000000000000000 ) ) ;
#11159 = EDGE_LOOP ( 'NONE', ( #2711, #5514, #9540, #2511 ) ) ;
#11160 = CARTESIAN_POINT ( 'NONE',  ( 2.121784821874994176, -23.98544242790896774, -3.566046559362932467 ) ) ;
#11161 = CARTESIAN_POINT ( 'NONE',  ( 2.115076519116362963, 31.37180007765647716, -3.012182706137107147 ) ) ;
#11162 = CIRCLE ( 'NONE', #15079, 2.149999999999995470 ) ;
#11163 = AXIS2_PLACEMENT_3D ( 'NONE', #2398, #6730, #9607 ) ;
#11164 = CYLINDRICAL_SURFACE ( 'NONE', #11876, 0.9999999999999991118 ) ;
#11165 = DIRECTION ( 'NONE',  ( -0.000000000000000000, 1.000000000000000000, -0.000000000000000000 ) ) ;
#11166 = DIRECTION ( 'NONE',  ( 0.000000000000000000, 0.000000000000000000, -1.000000000000000000 ) ) ;
#11167 = CARTESIAN_POINT ( 'NONE',  ( -4.648177544792955347E-16, -29.77410042770280185, -11.26655492845805107 ) ) ;
#11168 = CARTESIAN_POINT ( 'NONE',  ( 3.604268994871579590, -24.91053875026183562, -15.69445619563776617 ) ) ;
#11169 = CLOSED_SHELL ( 'NONE', ( #5225, #12379, #6480, #6610, #12582, #16360, #11186, #6545, #15031, #6432 ) ) ;
#11170 = CARTESIAN_POINT ( 'NONE',  ( -2.121784821875005722, -28.90027551689194496, -10.58515563886426136 ) ) ;
#11171 = ORIENTED_EDGE ( 'NONE', *, *, #15380, .T. ) ;
#11172 = DIRECTION ( 'NONE',  ( -4.915049848600951133E-16, 0.000000000000000000, -1.000000000000000000 ) ) ;
#11173 = CARTESIAN_POINT ( 'NONE',  ( 4.000000000000000888, -22.10963251316630362, -7.294347536058173098 ) ) ;
#11174 = VECTOR ( 'NONE', #17963, 1000.000000000000000 ) ;
#11175 = CARTESIAN_POINT ( 'NONE',  ( -0.05938372350927861171, 38.62180007765648071, -3.680117784833935701 ) ) ;
#11176 = AXIS2_PLACEMENT_3D ( 'NONE', #5503, #9669, #6973 ) ;
#11177 = VERTEX_POINT ( 'NONE', #5252 ) ;
#11178 = CARTESIAN_POINT ( 'NONE',  ( -4.000000000000000888, -22.23868721134528670, -7.478656746023200519 ) ) ;
#11179 = EDGE_CURVE ( 'NONE', #8695, #2685, #9099, .T. ) ;
#11180 = CARTESIAN_POINT ( 'NONE',  ( 1.444289557196047680, 17.24680007765648071, 4.262301884875704161 ) ) ;
#11181 = CARTESIAN_POINT ( 'NONE',  ( -4.000000000000000888, -20.36739408704506715, -4.806173200523589095 ) ) ;
#11182 = CARTESIAN_POINT ( 'NONE',  ( 0.7188294034286553114, 36.25319992234354771, 2.395093729190349130 ) ) ;
#11183 = VERTEX_POINT ( 'NONE', #9510 ) ;
#11184 = CARTESIAN_POINT ( 'NONE',  ( -4.243569643749998122, -22.94726928300757862, -12.76210693092232162 ) ) ;
#11185 = CARTESIAN_POINT ( 'NONE',  ( 1.444289557196047680, 29.74680007765648071, 4.262301884875704161 ) ) ;
#11186 = ADVANCED_FACE ( 'NONE', ( #15189 ), #1706, .T. ) ;
#11187 = ORIENTED_EDGE ( 'NONE', *, *, #5587, .T. ) ;
#11188 = CIRCLE ( 'NONE', #15951, 4.000000000000000000 ) ;
#11189 = DIRECTION ( 'NONE',  ( -0.000000000000000000, -0.5735764363510414965, -0.8191520442889950182 ) ) ;
#11190 = AXIS2_PLACEMENT_3D ( 'NONE', #11572, #5, #11669 ) ;
#11191 = CIRCLE ( 'NONE', #4685, 0.9999999999999991118 ) ;
#11192 = SURFACE_STYLE_FILL_AREA ( #12312 ) ;
#11193 = CARTESIAN_POINT ( 'NONE',  ( 8.500000000000019540, 0.000000000000000000, 18.49999999999998934 ) ) ;
#11194 = LINE ( 'NONE', #4158, #16283 ) ;
#11195 =( BOUNDED_CURVE ( )  B_SPLINE_CURVE ( 2, ( #162, #9973, #5992, #14349, #1649, #5813, #5901, #4422, #15743 ),
 .UNSPECIFIED., .F., .T. ) 
 B_SPLINE_CURVE_WITH_KNOTS ( ( 3, 2, 2, 2, 3 ),
 ( 0.5775862068965517127, 0.5804597701149425415, 0.5862068965517240882, 0.5919540229885057459, 0.5948275862068965747 ),
 .UNSPECIFIED. ) 
 CURVE ( )  GEOMETRIC_REPRESENTATION_ITEM ( )  RATIONAL_B_SPLINE_CURVE ( ( 0.9330127018922194093, 0.9330127018922194093, 1.000000000000000000, 0.8660254037844387076, 1.000000000000000000, 0.8660254037844387076, 1.000000000000000000, 0.9330127018922194093, 0.9330127018922194093 ) ) 
 REPRESENTATION_ITEM ( '' )  );
#11196 = CARTESIAN_POINT ( 'NONE',  ( 4.243569643750000786, -22.22255537372044998, -7.455618094274186092 ) ) ;
#11197 = VERTEX_POINT ( 'NONE', #8122 ) ;
#11198 = DIRECTION ( 'NONE',  ( 0.000000000000000000, -1.000000000000000000, 0.000000000000000000 ) ) ;
#11199 = EDGE_LOOP ( 'NONE', ( #15328, #7554, #10334 ) ) ;
#11200 = CARTESIAN_POINT ( 'NONE',  ( -1.999999999999996225, -21.76706409162843059, -12.84458598828390130 ) ) ;
#11201 = CARTESIAN_POINT ( 'NONE',  ( 0.000000000000000000, -10.00000000000000178, -12.59063537424807677 ) ) ;
#11202 = DIRECTION ( 'NONE',  ( 0.000000000000000000, 0.000000000000000000, -1.000000000000000000 ) ) ;
#11203 = SURFACE_SIDE_STYLE ('',( #5555 ) ) ;
#11204 = CARTESIAN_POINT ( 'NONE',  ( 3.673772985318163098, 20.50319992234354771, -2.599342558261029001 ) ) ;
#11205 = CARTESIAN_POINT ( 'NONE',  ( 0.05938372350920110426, 17.62819992234354771, -3.680117784833935701 ) ) ;
#11206 = CIRCLE ( 'NONE', #12094, 0.9999999999999991118 ) ;
#11207 = CARTESIAN_POINT ( 'NONE',  ( 4.713407268011036227E-15, -22.39135427958444069, -15.74932372938122427 ) ) ;
#11208 = CARTESIAN_POINT ( 'NONE',  ( 2.518350579753628971, 36.87180007765648071, 0.7558219633769073242 ) ) ;
#11209 = CARTESIAN_POINT ( 'NONE',  ( 2.829195390882724759, 27.87819992234354416, -3.793023760679264278 ) ) ;
#11210 = CARTESIAN_POINT ( 'NONE',  ( 2.000000000000004441, -20.71311738912845257, -11.33939410589610652 ) ) ;
#11211 = VERTEX_POINT ( 'NONE', #7178 ) ;
#11212 = CARTESIAN_POINT ( 'NONE',  ( -4.243569643749997233, -18.55940954492211503, -6.495593792111509224 ) ) ;
#11213 = CARTESIAN_POINT ( 'NONE',  ( 2.115076519116362963, 18.87180007765648071, -3.012182706137107147 ) ) ;
#11214 = FACE_OUTER_BOUND ( 'NONE', #6720, .T. ) ;
#11215 = AXIS2_PLACEMENT_3D ( 'NONE', #16855, #6989, #8119 ) ;
#11216 = CARTESIAN_POINT ( 'NONE',  ( 4.730628863548789710E-15, -19.40242359420666318, -11.97103273789424449 ) ) ;
#11217 = AXIS2_PLACEMENT_3D ( 'NONE', #16608, #1022, #9532 ) ;
#11218 = ADVANCED_FACE ( 'NONE', ( #17127 ), #16219, .T. ) ;
#11219 = CARTESIAN_POINT ( 'NONE',  ( 1.533898589781675205E-14, -28.03186200299146336, -8.778380594936995962 ) ) ;
#11220 = CARTESIAN_POINT ( 'NONE',  ( 3.999999999999996447, -24.21647428920293876, -6.276911511947378841 ) ) ;
#11221 = CARTESIAN_POINT ( 'NONE',  ( 9.000000000000001776, 40.79999999999999716, -2.500000000000002665 ) ) ;
#11222 = EDGE_LOOP ( 'NONE', ( #10752, #11394, #2108, #13494 ) ) ;
#11223 = ORIENTED_EDGE ( 'NONE', *, *, #18203, .T. ) ;
#11224 = CARTESIAN_POINT ( 'NONE',  ( 3.481649420246369697, 24.12180007765648071, -1.193696214020541824 ) ) ;
#11225 = EDGE_CURVE ( 'NONE', #1579, #15990, #11762, .T. ) ;
#11226 = DIRECTION ( 'NONE',  ( 0.000000000000000000, 0.8191520442889952403, -0.5735764363510413855 ) ) ;
#11227 = FACE_OUTER_BOUND ( 'NONE', #12273, .T. ) ;
#11228 = DIRECTION ( 'NONE',  ( -0.000000000000000000, 1.000000000000000000, -0.000000000000000000 ) ) ;
#11229 = VERTEX_POINT ( 'NONE', #11083 ) ;
#11230 = CARTESIAN_POINT ( 'NONE',  ( 3.481649420246394122, 15.87819992234354594, 1.193696214020467439 ) ) ;
#11231 = CARTESIAN_POINT ( 'NONE',  ( -4.243569643749997233, -21.36634923031502353, -10.50431910885077791 ) ) ;
#11232 = CARTESIAN_POINT ( 'NONE',  ( 3.518350579753631191, 31.87180007765647716, 1.080741659609802285 ) ) ;
#11233 = AXIS2_PLACEMENT_3D ( 'NONE', #12409, #5545, #2695 ) ;
#11234 = CARTESIAN_POINT ( 'NONE',  ( 2.798362969681409851, 26.00319992234354771, 2.102939460078764977 ) ) ;
#11235 = CARTESIAN_POINT ( 'NONE',  ( 15.00000000000000355, -4.000000000000000000, 30.00000000000000000 ) ) ;
#11236 = CYLINDRICAL_SURFACE ( 'NONE', #1659, 4.000000000000000000 ) ;
#11237 = CARTESIAN_POINT ( 'NONE',  ( 4.730628863548789710E-15, -19.43468726875141073, -12.01711004038550001 ) ) ;
#11238 = DIRECTION ( 'NONE',  ( -0.000000000000000000, 0.5000000000000000000, 0.8660254037844385966 ) ) ;
#11239 = EDGE_CURVE ( 'NONE', #10567, #1717, #5617, .T. ) ;
#11240 = EDGE_CURVE ( 'NONE', #4895, #1346, #8654, .T. ) ;
#11241 = AXIS2_PLACEMENT_3D ( 'NONE', #16007, #7457, #5791 ) ;
#11242 = DIRECTION ( 'NONE',  ( -1.000000000000000000, 0.000000000000000000, 4.336808689942021680E-16 ) ) ;
#11243 = ADVANCED_FACE ( 'NONE', ( #4228 ), #6437, .T. ) ;
#11244 = DIRECTION ( 'NONE',  ( -0.000000000000000000, -1.000000000000000000, -0.000000000000000000 ) ) ;
#11245 = CARTESIAN_POINT ( 'NONE',  ( 4.730628863548789710E-15, -17.07943902698494298, -8.653466958523816643 ) ) ;
#11246 = DIRECTION ( 'NONE',  ( -0.000000000000000000, -0.5735764363510414965, -0.8191520442889950182 ) ) ;
#11247 = DIRECTION ( 'NONE',  ( -0.000000000000000000, 1.000000000000000000, -0.000000000000000000 ) ) ;
#11248 = ORIENTED_EDGE ( 'NONE', *, *, #13460, .F. ) ;
#11249 = CARTESIAN_POINT ( 'NONE',  ( -1.593127413382998459, 38.37180007765647360, -2.091722143975139669 ) ) ;
#11250 = CARTESIAN_POINT ( 'NONE',  ( -1.071796769724496334, -25.39776739033617048, -5.016503624303159548 ) ) ;
#11251 = CARTESIAN_POINT ( 'NONE',  ( 4.898587196589413815E-16, 2.700915433685006750, 35.11257424290206330 ) ) ;
#11252 = CARTESIAN_POINT ( 'NONE',  ( -9.000000000000003553, 40.79999999999999716, -2.500000000000001776 ) ) ;
#11253 = ORIENTED_EDGE ( 'NONE', *, *, #12494, .T. ) ;
#11254 = CARTESIAN_POINT ( 'NONE',  ( 4.243569643750000786, -20.67389899557263533, -5.243907574693898788 ) ) ;
#11255 = AXIS2_PLACEMENT_3D ( 'NONE', #6045, #7062, #7339 ) ;
#11256 = CARTESIAN_POINT ( 'NONE',  ( 3.518350579753631191, 31.87180007765647716, 1.080741659609802285 ) ) ;
#11257 =( LENGTH_UNIT ( ) NAMED_UNIT ( * ) SI_UNIT ( .MILLI., .METRE. ) );
#11258 = CARTESIAN_POINT ( 'NONE',  ( 4.000000000000000000, 3.518949890710770134, -4.119968255444916849E-15 ) ) ;
#11259 = LINE ( 'NONE', #4225, #10550 ) ;
#11260 = CARTESIAN_POINT ( 'NONE',  ( -4.000000000000004441, -24.30251075465558586, -6.399784318590733712 ) ) ;
#11261 = CARTESIAN_POINT ( 'NONE',  ( 8.499999999999994671, 15.00000000000000178, 18.35000000000000142 ) ) ;
#11262 = CARTESIAN_POINT ( 'NONE',  ( 2.121784821874994176, -29.63158547323952874, -11.62957449533272580 ) ) ;
#11263 = VERTEX_POINT ( 'NONE', #2671 ) ;
#11264 = CARTESIAN_POINT ( 'NONE',  ( -2.000000000000005773, -26.51742392663723180, -7.549849196723933176 ) ) ;
#11265 = CARTESIAN_POINT ( 'NONE',  ( -4.000000000000000888, -21.72246841862934730, -6.741419906163105047 ) ) ;
#11266 = AXIS2_PLACEMENT_3D ( 'NONE', #17513, #7460, #13024 ) ;
#11267 = CARTESIAN_POINT ( 'NONE',  ( 2.211161402132902243, 39.62180007765646650, 2.942372952327172442 ) ) ;
#11268 = ORIENTED_EDGE ( 'NONE', *, *, #6329, .T. ) ;
#11269 = CARTESIAN_POINT ( 'NONE',  ( -1.071796769724486786, -19.01507968255996417, -9.848655261753959778 ) ) ;
#11270 = EDGE_CURVE ( 'NONE', #13588, #15144, #10276, .T. ) ;
#11271 = APPLICATION_PROTOCOL_DEFINITION ( 'draft international standard', 'automotive_design', 1998, #7837 ) ;
#11272 = DIRECTION ( 'NONE',  ( -1.000000000000000000, 0.000000000000000000, 0.000000000000000000 ) ) ;
#11273 = CARTESIAN_POINT ( 'NONE',  ( -2.500000000000001332, 37.00319992234354771, -0.05647727720530596601 ) ) ;
#11274 = ORIENTED_EDGE ( 'NONE', *, *, #8295, .F. ) ;
#11275 = CARTESIAN_POINT ( 'NONE',  ( 4.243569643750000786, -25.57797752637403832, -12.24765755336480666 ) ) ;
#11276 = CARTESIAN_POINT ( 'NONE',  ( -4.481649420246366589, 35.37180007765647360, 1.518615910253458878 ) ) ;
#11277 = ORIENTED_EDGE ( 'NONE', *, *, #4375, .T. ) ;
#11278 = CARTESIAN_POINT ( 'NONE',  ( -1.071796769724486564, -27.26906051463638647, -7.688987169802764754 ) ) ;
#11279 = DIRECTION ( 'NONE',  ( -1.000000000000000000, -0.000000000000000000, -0.000000000000000000 ) ) ;
#11280 = DIRECTION ( 'NONE',  ( -1.000000000000000000, -0.000000000000000000, -0.000000000000000000 ) ) ;
#11281 = CARTESIAN_POINT ( 'NONE',  ( 4.243569643749996345, -25.02533654799221097, -7.186914330003371099 ) ) ;
#11282 = EDGE_CURVE ( 'NONE', #8773, #9873, #825, .T. ) ;
#11283 = EDGE_LOOP ( 'NONE', ( #13893, #15056 ) ) ;
#11284 = DIRECTION ( 'NONE',  ( 0.000000000000000000, 0.000000000000000000, -1.000000000000000000 ) ) ;
#11285 = ORIENTED_EDGE ( 'NONE', *, *, #13407, .F. ) ;
#11286 = CARTESIAN_POINT ( 'NONE',  ( -4.000000000000004441, -25.91569448259783215, -8.703649444160298287 ) ) ;
#11287 = CARTESIAN_POINT ( 'NONE',  ( 0.000000000000000000, 5.977523610840987267, 32.81826849749789687 ) ) ;
#11288 = EDGE_CURVE ( 'NONE', #13336, #451, #143, .T. ) ;
#11289 = CARTESIAN_POINT ( 'NONE',  ( -5.577813053751546416E-15, -28.99977223862889275, -10.16069966866791141 ) ) ;
#11290 = CARTESIAN_POINT ( 'NONE',  ( 4.481649420246397675, 18.37819992234354416, 1.518615910253363177 ) ) ;
#11291 = CARTESIAN_POINT ( 'NONE',  ( 2.211161402132839182, 22.87819992234354416, -2.942372952327217739 ) ) ;
#11292 = CARTESIAN_POINT ( 'NONE',  ( 4.713407268011036227E-15, -22.64946367594241039, -16.11794214931127556 ) ) ;
#11293 = CARTESIAN_POINT ( 'NONE',  ( -1.497042530366477164, 40.12180007765647360, 2.161531897785062384 ) ) ;
#11294 = CARTESIAN_POINT ( 'NONE',  ( -3.607379964056363075, 32.25319992234354061, -2.690724712371229899 ) ) ;
#11295 = CARTESIAN_POINT ( 'NONE',  ( -1.999999999999996225, -20.41198976004415044, -10.90933928264438890 ) ) ;
#11296 = VERTEX_POINT ( 'NONE', #14143 ) ;
#11297 = CIRCLE ( 'NONE', #14011, 6.500000000000000000 ) ;
#11298 = CARTESIAN_POINT ( 'NONE',  ( 12.00000000000000178, 13.00000000000000178, 15.00000000000000000 ) ) ;
#11299 = CIRCLE ( 'NONE', #3330, 8.000000000000001776 ) ;
#11300 = CARTESIAN_POINT ( 'NONE',  ( -3.500000000000000444, 20.49680007765647716, 0.05647727720536892260 ) ) ;
#11301 =( BOUNDED_CURVE ( )  B_SPLINE_CURVE ( 2, ( #8502, #1660, #15660, #365, #3143, #13053, #14268, #5645, #14080 ),
 .UNSPECIFIED., .F., .F. ) 
 B_SPLINE_CURVE_WITH_KNOTS ( ( 3, 2, 2, 2, 3 ),
 ( 0.8706896551724138122, 0.8735632183908046411, 0.8793103448275861878, 0.8850574712643678454, 0.8879310344827586743 ),
 .UNSPECIFIED. ) 
 CURVE ( )  GEOMETRIC_REPRESENTATION_ITEM ( )  RATIONAL_B_SPLINE_CURVE ( ( 0.9330127018922194093, 0.9330127018922194093, 1.000000000000000000, 0.8660254037844387076, 1.000000000000000000, 0.8660254037844387076, 1.000000000000000000, 0.9330127018922180770, 0.9330127018922194093 ) ) 
 REPRESENTATION_ITEM ( '' )  );
#11302 = CARTESIAN_POINT ( 'NONE',  ( -9.566989785610495289, -9.974423619177718692, -0.6215033074179308059 ) ) ;
#11303 = CARTESIAN_POINT ( 'NONE',  ( 4.243569643750003451, -21.19427629940971869, -10.25857349556407527 ) ) ;
#11304 = CARTESIAN_POINT ( 'NONE',  ( -0.05938372350928957516, 26.12180007765648426, -4.731580009072201776 ) ) ;
#11305 = DIRECTION ( 'NONE',  ( -0.000000000000000000, -1.000000000000000000, -0.000000000000000000 ) ) ;
#11306 = CARTESIAN_POINT ( 'NONE',  ( -2.000000000000005773, -26.06573248371572760, -6.904766962853115864 ) ) ;
#11307 = EDGE_CURVE ( 'NONE', #6836, #5293, #10046, .T. ) ;
#11308 = ORIENTED_EDGE ( 'NONE', *, *, #15246, .T. ) ;
#11309 = ORIENTED_EDGE ( 'NONE', *, *, #8190, .F. ) ;
#11310 = CARTESIAN_POINT ( 'NONE',  ( -1.135272562821090014, 25.99680007765648071, -3.311245368580554072 ) ) ;
#11311 = DIRECTION ( 'NONE',  ( 0.000000000000000000, 0.000000000000000000, -1.000000000000000000 ) ) ;
#11312 = DIRECTION ( 'NONE',  ( 1.000000000000000000, 0.000000000000000000, 0.000000000000000000 ) ) ;
#11313 = CIRCLE ( 'NONE', #3344, 2.000000000000001776 ) ;
#11314 = DIRECTION ( 'NONE',  ( -0.000000000000000000, -1.000000000000000000, -0.000000000000000000 ) ) ;
#11315 = ORIENTED_EDGE ( 'NONE', *, *, #103, .T. ) ;
#11316 = AXIS2_PLACEMENT_3D ( 'NONE', #14747, #9069, #7490 ) ;
#11317 = CARTESIAN_POINT ( 'NONE',  ( -2.211161402132839182, 21.62819992234354771, 2.942372952327218627 ) ) ;
#11318 = CARTESIAN_POINT ( 'NONE',  ( 4.730628863548789710E-15, -18.36998600877478438, -10.49655905817405355 ) ) ;
#11319 = CARTESIAN_POINT ( 'NONE',  ( 1.497042530366477164, 16.37180007765648426, -2.161531897785062384 ) ) ;
#11320 = CARTESIAN_POINT ( 'NONE',  ( 2.211161402132839626, 35.37819992234353350, -2.942372952327218183 ) ) ;
#11321 = DIRECTION ( 'NONE',  ( -1.000000000000000000, -0.000000000000000000, -0.000000000000000000 ) ) ;
#11322 = CYLINDRICAL_SURFACE ( 'NONE', #8101, 0.9999999999999991118 ) ;
#11323 = CARTESIAN_POINT ( 'NONE',  ( 4.730628863548789710E-15, -18.14414028696156933, -10.17401794073526311 ) ) ;
#11324 = CIRCLE ( 'NONE', #9849, 1.250000000000000222 ) ;
#11325 = CIRCLE ( 'NONE', #11046, 10.00000000000000000 ) ;
#11326 = FACE_OUTER_BOUND ( 'NONE', #8711, .T. ) ;
#11327 = CARTESIAN_POINT ( 'NONE',  ( -8.000000000000001776, 40.79999999999999716, 2.499999999999995115 ) ) ;
#11328 = DIRECTION ( 'NONE',  ( 0.000000000000000000, 0.000000000000000000, -1.000000000000000000 ) ) ;
#11329 =( BOUNDED_CURVE ( )  B_SPLINE_CURVE ( 2, ( #10012, #14294, #1596, #7229, #6962, #4460, #1330, #7049, #8359 ),
 .UNSPECIFIED., .F., .T. ) 
 B_SPLINE_CURVE_WITH_KNOTS ( ( 3, 2, 2, 2, 3 ),
 ( 0.7327586206896552490, 0.7356321839080459668, 0.7413793103448276245, 0.7471264367816091712, 0.7500000000000000000 ),
 .UNSPECIFIED. ) 
 CURVE ( )  GEOMETRIC_REPRESENTATION_ITEM ( )  RATIONAL_B_SPLINE_CURVE ( ( 0.9330127018922194093, 0.9330127018922206306, 1.000000000000000000, 0.8660254037844387076, 1.000000000000000000, 0.8660254037844387076, 1.000000000000000000, 0.9330127018922194093, 0.9330127018922194093 ) ) 
 REPRESENTATION_ITEM ( '' )  );
#11330 = CARTESIAN_POINT ( 'NONE',  ( 4.730628863548789710E-15, -16.56322023426900714, -7.916230118663721171 ) ) ;
#11331 = CARTESIAN_POINT ( 'NONE',  ( -1.318039840154427544, 15.00000000000000178, -3.027868313707952730 ) ) ;
#11332 = ORIENTED_EDGE ( 'NONE', *, *, #9430, .T. ) ;
#11333 = CARTESIAN_POINT ( 'NONE',  ( 2.055738996568281518, 23.00319992234354771, -1.423772053676066518 ) ) ;
#11334 = CARTESIAN_POINT ( 'NONE',  ( 3.579096709490575479E-14, -26.67678767140717966, -6.843133889297480899 ) ) ;
#11335 = CARTESIAN_POINT ( 'NONE',  ( -2.864755990943265829, 18.24680007765648071, -2.011557305968488141 ) ) ;
#11336 = AXIS2_PLACEMENT_3D ( 'NONE', #6075, #9138, #3311 ) ;
#11337 = CARTESIAN_POINT ( 'NONE',  ( 8.000000000000000000, 31.99999999999999289, -2.500000000000000888 ) ) ;
#11338 = DIRECTION ( 'NONE',  ( -1.000000000000000000, 0.000000000000000000, 0.000000000000000000 ) ) ;
#11339 = EDGE_CURVE ( 'NONE', #13916, #10922, #5546, .T. ) ;
#11340 = ORIENTED_EDGE ( 'NONE', *, *, #8693, .T. ) ;
#11341 = CARTESIAN_POINT ( 'NONE',  ( -1.734723475976807094E-15, 20.99999999999999289, -2.500000000000000000 ) ) ;
#11342 = CARTESIAN_POINT ( 'NONE',  ( 3.500000000000000444, 29.24680007765647716, -0.05647727720536935281 ) ) ;
#11343 = EDGE_CURVE ( 'NONE', #18081, #5029, #12751, .T. ) ;
#11344 = EDGE_CURVE ( 'NONE', #17654, #11263, #12649, .T. ) ;
#11345 = CARTESIAN_POINT ( 'NONE',  ( 13.00000000000000178, 49.00000000000000000, -16.00000000000000000 ) ) ;
#11346 = CARTESIAN_POINT ( 'NONE',  ( -4.243569643750000786, -25.41665915365029704, -12.01727104090852905 ) ) ;
#11347 = DIRECTION ( 'NONE',  ( 0.000000000000000000, 1.000000000000000000, 0.000000000000000000 ) ) ;
#11348 = EDGE_CURVE ( 'NONE', #4578, #10649, #15631, .T. ) ;
#11349 = DIRECTION ( 'NONE',  ( 0.000000000000000000, -0.5000000000000002220, 0.8660254037844384856 ) ) ;
#11350 = DIRECTION ( 'NONE',  ( 0.000000000000000000, 0.000000000000000000, -1.000000000000000000 ) ) ;
#11351 = CARTESIAN_POINT ( 'NONE',  ( -2.121784821874996396, -21.67493339405068653, -13.08076802302275077 ) ) ;
#11352 = ORIENTED_EDGE ( 'NONE', *, *, #17501, .F. ) ;
#11353 = DIRECTION ( 'NONE',  ( -0.000000000000000000, -1.000000000000000000, -0.000000000000000000 ) ) ;
#11354 = CARTESIAN_POINT ( 'NONE',  ( -3.999999999999997335, -18.30357054373476444, -5.885045627956057679 ) ) ;
#11355 = CARTESIAN_POINT ( 'NONE',  ( -1.497042530366477164, 25.12180007765648071, 2.161531897785062384 ) ) ;
#11356 = EDGE_LOOP ( 'NONE', ( #10711, #10283, #7386, #1414 ) ) ;
#11357 = EDGE_CURVE ( 'NONE', #4590, #3584, #6910, .T. ) ;
#11358 = CYLINDRICAL_SURFACE ( 'NONE', #14898, 4.000000000000000000 ) ;
#11359 = CARTESIAN_POINT ( 'NONE',  ( -3.999999999999997335, -21.14277390367241694, -9.939848247186583663 ) ) ;
#11360 = CARTESIAN_POINT ( 'NONE',  ( -0.8262555684460826111, 36.50319992234354061, 2.360188852285421302 ) ) ;
#11361 = ORIENTED_EDGE ( 'NONE', *, *, #18236, .T. ) ;
#11362 = CARTESIAN_POINT ( 'NONE',  ( 2.121784821875004390, -21.75021530132177006, -13.18828172883567973 ) ) ;
#11363 = CARTESIAN_POINT ( 'NONE',  ( -1.444289557196047014, 30.99680007765647716, -4.262301884875704161 ) ) ;
#11364 = VERTEX_POINT ( 'NONE', #1361 ) ;
#11365 = CARTESIAN_POINT ( 'NONE',  ( 0.000000000000000000, 5.977523610840987267, 32.81826849749789687 ) ) ;
#11366 = AXIS2_PLACEMENT_3D ( 'NONE', #13590, #3949, #905 ) ;
#11367 = CARTESIAN_POINT ( 'NONE',  ( 4.000000000000003553, -18.13149761282945605, -5.639300014669354155 ) ) ;
#11368 = PLANE ( 'NONE',  #11411 ) ;
#11369 = DIRECTION ( 'NONE',  ( -0.000000000000000000, 1.000000000000000000, -0.000000000000000000 ) ) ;
#11370 = CARTESIAN_POINT ( 'NONE',  ( 3.999999999999996447, -28.08811523457247006, -11.80618781089809488 ) ) ;
#11371 = CARTESIAN_POINT ( 'NONE',  ( -2.121784821874996396, -18.86799370865777803, -9.072042706283481195 ) ) ;
#11372 = ORIENTED_EDGE ( 'NONE', *, *, #8930, .F. ) ;
#11373 =( REPRESENTATION_RELATIONSHIP ('NONE','NONE', #15868, #1416 ) REPRESENTATION_RELATIONSHIP_WITH_TRANSFORMATION ( #8201 )SHAPE_REPRESENTATION_RELATIONSHIP( ) );
#11374 = CARTESIAN_POINT ( 'NONE',  ( 1.533898589781675205E-14, -27.96733465319702105, -8.686225988947720467 ) ) ;
#11375 = ORIENTED_EDGE ( 'NONE', *, *, #17147, .T. ) ;
#11376 = VERTEX_POINT ( 'NONE', #5709 ) ;
#11377 = DIRECTION ( 'NONE',  ( 0.000000000000000000, 1.000000000000000000, -1.224646799147353207E-16 ) ) ;
#11378 = DIRECTION ( 'NONE',  ( 0.000000000000000000, 0.000000000000000000, 1.000000000000000000 ) ) ;
#11379 =( NAMED_UNIT ( * ) PLANE_ANGLE_UNIT ( ) SI_UNIT ( $, .RADIAN. ) );
#11380 = CARTESIAN_POINT ( 'NONE',  ( -1.444289557195956863, 19.00319992234354771, 4.262301884875733471 ) ) ;
#11381 = CARTESIAN_POINT ( 'NONE',  ( -0.05938372350920064630, 31.37819992234354416, 3.680117784833935701 ) ) ;
#11382 = CARTESIAN_POINT ( 'NONE',  ( 4.000000000000003553, -23.80990433270476458, -13.74890525313040612 ) ) ;
#11383 = CARTESIAN_POINT ( 'NONE',  ( 1.497042530366477164, 36.37180007765648071, -2.161531897785062384 ) ) ;
#11384 = CARTESIAN_POINT ( 'NONE',  ( -2.733110507866328476, 37.37819992234354771, -3.862833514489096398 ) ) ;
#11385 = CARTESIAN_POINT ( 'NONE',  ( 4.000000000000000888, -23.59376154151967953, -9.413903449649181354 ) ) ;
#11386 = ORIENTED_EDGE ( 'NONE', *, *, #8030, .T. ) ;
#11387 = DIRECTION ( 'NONE',  ( -0.000000000000000000, -0.5735764363510414965, -0.8191520442889950182 ) ) ;
#11388 = CARTESIAN_POINT ( 'NONE',  ( -1.027846397803541700, 24.99680007765647716, 3.346150245485522312 ) ) ;
#11389 = CARTESIAN_POINT ( 'NONE',  ( 9.324435358932730011, -9.992494772396325331, -2.158019202327493336 ) ) ;
#11390 = CARTESIAN_POINT ( 'NONE',  ( -4.243569643750000786, -22.57745579371264455, -7.962468421678005726 ) ) ;
#11391 = CARTESIAN_POINT ( 'NONE',  ( 3.673772985318219053, 29.49680007765647360, 2.599342558260951730 ) ) ;
#11392 = CYLINDRICAL_SURFACE ( 'NONE', #4157, 6.499999999999999112 ) ;
#11393 = CARTESIAN_POINT ( 'NONE',  ( 0.000000000000000000, 13.00000000000000178, 0.000000000000000000 ) ) ;
#11394 = ORIENTED_EDGE ( 'NONE', *, *, #2209, .T. ) ;
#11395 = ORIENTED_EDGE ( 'NONE', *, *, #9827, .F. ) ;
#11396 = CARTESIAN_POINT ( 'NONE',  ( 0.05938372350927906274, 22.37180007765648071, 3.680117784833935701 ) ) ;
#11397 = CARTESIAN_POINT ( 'NONE',  ( -9.000000000000001776, 36.39999999999999147, 2.499999999999995559 ) ) ;
#11398 = CARTESIAN_POINT ( 'NONE',  ( -1.999999999999996225, -23.31572046977624169, -15.05629650786418772 ) ) ;
#11399 = CARTESIAN_POINT ( 'NONE',  ( 10.00000000000000355, 18.79999999999999361, 2.499999999999996891 ) ) ;
#11400 = EDGE_LOOP ( 'NONE', ( #3334, #4891 ) ) ;
#11401 = CARTESIAN_POINT ( 'NONE',  ( -1.027846397803611866, 17.50319992234354416, -3.346150245485499219 ) ) ;
#11402 = CARTESIAN_POINT ( 'NONE',  ( -4.243569643749997233, -20.33391164488314828, -9.029845429130588741 ) ) ;
#11403 = CARTESIAN_POINT ( 'NONE',  ( -1.027846397803541700, 37.49680007765647360, 3.346150245485522312 ) ) ;
#11404 = CIRCLE ( 'NONE', #3720, 2.200000000000000178 ) ;
#11405 = CARTESIAN_POINT ( 'NONE',  ( -2.211161402132839182, 36.62819992234354771, 2.942372952327218627 ) ) ;
#11406 = CARTESIAN_POINT ( 'NONE',  ( -13.00000000000000178, 13.00000000000000178, -25.00000000000000355 ) ) ;
#11407 = DIRECTION ( 'NONE',  ( -0.000000000000000000, 1.000000000000000000, -0.000000000000000000 ) ) ;
#11408 =( BOUNDED_CURVE ( )  B_SPLINE_CURVE ( 2, ( #8809, #5849, #11495, #17472, #17190, #4463, #12985, #299, #14490 ),
 .UNSPECIFIED., .F., .T. ) 
 B_SPLINE_CURVE_WITH_KNOTS ( ( 3, 2, 2, 2, 3 ),
 ( 0.07758620689655172653, 0.08045977011494252762, 0.08620689655172414367, 0.09195402298850574585, 0.09482758620689656082 ),
 .UNSPECIFIED. ) 
 CURVE ( )  GEOMETRIC_REPRESENTATION_ITEM ( )  RATIONAL_B_SPLINE_CURVE ( ( 0.9330127018922194093, 0.9330127018922194093, 1.000000000000000000, 0.8660254037844387076, 1.000000000000000000, 0.8660254037844387076, 1.000000000000000000, 0.9330127018922191873, 0.9330127018922194093 ) ) 
 REPRESENTATION_ITEM ( '' )  );
#11409 = CARTESIAN_POINT ( 'NONE',  ( 2.121784821875004390, -19.94344952681598926, -10.60795278932534558 ) ) ;
#11410 = EDGE_CURVE ( 'NONE', #7842, #16544, #17039, .T. ) ;
#11411 = AXIS2_PLACEMENT_3D ( 'NONE', #8585, #17058, #15484 ) ;
#11412 = CARTESIAN_POINT ( 'NONE',  ( -2.649389826664908298, -10.00000000000000178, -4.175485738723567763 ) ) ;
#11413 = CARTESIAN_POINT ( 'NONE',  ( -5.577813053751546416E-15, -23.90211166126395881, -2.880485876056233518 ) ) ;
#11414 = CARTESIAN_POINT ( 'NONE',  ( -8.500000000000005329, 10.00000000000000000, -20.49999999999999645 ) ) ;
#11415 = CARTESIAN_POINT ( 'NONE',  ( 2.121784821874994176, -23.43695996064828435, -2.782732417011581028 ) ) ;
#11416 = CLOSED_SHELL ( 'NONE', ( #10432, #16185, #12324, #721, #14549, #225, #2214, #14493, #10933, #14552 ) ) ;
#11417 = CARTESIAN_POINT ( 'NONE',  ( -8.500000000000005329, 15.00000000000000178, -20.49999999999999645 ) ) ;
#11418 = DIRECTION ( 'NONE',  ( 0.000000000000000000, 0.000000000000000000, 1.000000000000000000 ) ) ;
#11419 = ORIENTED_EDGE ( 'NONE', *, *, #17831, .F. ) ;
#11420 = CARTESIAN_POINT ( 'NONE',  ( 2.518350579753611207, 20.62819992234354771, -0.7558219633769606149 ) ) ;
#11421 = AXIS2_PLACEMENT_3D ( 'NONE', #907, #2219, #5342 ) ;
#11422 = DIRECTION ( 'NONE',  ( 0.000000000000000000, 0.000000000000000000, -1.000000000000000000 ) ) ;
#11423 = CARTESIAN_POINT ( 'NONE',  ( -2.864755990943265829, 15.74680007765647716, -2.011557305968488141 ) ) ;
#11424 = DIRECTION ( 'NONE',  ( 0.000000000000000000, 0.000000000000000000, 1.000000000000000000 ) ) ;
#11425 = DIRECTION ( 'NONE',  ( -1.000000000000000000, -0.000000000000000000, -0.000000000000000000 ) ) ;
#11426 = VERTEX_POINT ( 'NONE', #18254 ) ;
#11427 = CARTESIAN_POINT ( 'NONE',  ( 4.730628863548789710E-15, -16.33737451245578498, -7.593689001224929847 ) ) ;
#11428 = CARTESIAN_POINT ( 'NONE',  ( 3.500000000000000444, 31.74680007765647716, -0.05647727720536935281 ) ) ;
#11429 = CARTESIAN_POINT ( 'NONE',  ( -2.000000000000005773, -22.64578298126770051, -2.020572897773216692 ) ) ;
#11430 = DIRECTION ( 'NONE',  ( 0.000000000000000000, -1.000000000000000000, 0.000000000000000000 ) ) ;
#11431 = AXIS2_PLACEMENT_3D ( 'NONE', #8723, #13181, #1798 ) ;
#11432 = CARTESIAN_POINT ( 'NONE',  ( 4.243569643750003451, -24.29158905570533733, -14.68199453472465521 ) ) ;
#11433 = FACE_OUTER_BOUND ( 'NONE', #11710, .T. ) ;
#11434 = PLANE ( 'NONE',  #16298 ) ;
#11435 = CARTESIAN_POINT ( 'NONE',  ( 14.99999999999999822, 13.00000000000000178, 24.99999999999999645 ) ) ;
#11436 = CARTESIAN_POINT ( 'NONE',  ( 2.121784821875004390, -22.23417041949295481, -13.87944126620451790 ) ) ;
#11437 = EDGE_CURVE ( 'NONE', #4809, #13013, #17734, .T. ) ;
#11438 = CARTESIAN_POINT ( 'NONE',  ( 1.300000000000000044, -0.7216878364870317197, 1.250000000000000000 ) ) ;
#11440 = EDGE_CURVE ( 'NONE', #4695, #18119, #7290, .T. ) ;
#11439 = CARTESIAN_POINT ( 'NONE',  ( 1.999999999999994449, -22.66729209833581749, -2.051291100440815640 ) ) ;
#11441 = CARTESIAN_POINT ( 'NONE',  ( 0.8262555684461332373, 22.24680007765648071, 2.360188852285403982 ) ) ;
#11442 = VERTEX_POINT ( 'NONE', #16188 ) ;
#11443 = CARTESIAN_POINT ( 'NONE',  ( 2.864755990943265829, 21.99680007765647716, 2.011557305968487697 ) ) ;
#11444 = CARTESIAN_POINT ( 'NONE',  ( 0.000000000000000000, 18.79999999999999361, 2.500000000000000000 ) ) ;
#11445 = SHAPE_REPRESENTATION_RELATIONSHIP ( 'NONE' , 'NONE' ,  #10770, #12694 ) ;
#11446 = DIRECTION ( 'NONE',  ( -0.000000000000000000, -1.000000000000000000, -0.000000000000000000 ) ) ;
#11447 = VECTOR ( 'NONE', #1653, 1000.000000000000000 ) ;
#11448 = CARTESIAN_POINT ( 'NONE',  ( 2.055738996568281518, 38.00319992234354061, -1.423772053676066518 ) ) ;
#11449 = VERTEX_POINT ( 'NONE', #11718 ) ;
#11450 = CARTESIAN_POINT ( 'NONE',  ( 2.121784821875004390, -21.23399650860583066, -12.45104488897558248 ) ) ;
#11451 = CARTESIAN_POINT ( 'NONE',  ( 1.444289557196047680, 34.74680007765647360, 4.262301884875704161 ) ) ;
#11452 = EDGE_LOOP ( 'NONE', ( #5549, #6172, #2863, #16060, #4612, #647 ) ) ;
#11453 = SURFACE_SIDE_STYLE ('',( #16969 ) ) ;
#11454 = CARTESIAN_POINT ( 'NONE',  ( -8.500000000000010658, 10.00000000000000000, 20.49999999999998934 ) ) ;
#11455 = CARTESIAN_POINT ( 'NONE',  ( 3.579096709490575479E-14, -24.61191250054342916, -3.894186529857098567 ) ) ;
#11456 = AXIS2_PLACEMENT_3D ( 'NONE', #16469, #15170, #3751 ) ;
#11457 = CARTESIAN_POINT ( 'NONE',  ( -13.00000000000000178, 15.00000000000000178, -25.00000000000000355 ) ) ;
#11459 = FACE_OUTER_BOUND ( 'NONE', #8691, .T. ) ;
#11458 = VECTOR ( 'NONE', #2284, 1000.000000000000000 ) ;
#11460 = CARTESIAN_POINT ( 'NONE',  ( -4.243569643750005227, -22.78838844622314497, -3.992221357276296345 ) ) ;
#11461 = EDGE_LOOP ( 'NONE', ( #14172, #10544, #14580, #4596 ) ) ;
#11462 = EDGE_CURVE ( 'NONE', #12907, #16218, #5576, .T. ) ;
#11463 = CARTESIAN_POINT ( 'NONE',  ( 4.000000000000000888, -23.07754274880374368, -8.676666609789087659 ) ) ;
#11464 = ADVANCED_FACE ( 'NONE', ( #15911 ), #17121, .T. ) ;
#11465 = ORIENTED_EDGE ( 'NONE', *, *, #14526, .F. ) ;
#11466 = ORIENTED_EDGE ( 'NONE', *, *, #4085, .F. ) ;
#11467 = DIRECTION ( 'NONE',  ( -3.373073425510457965E-16, 0.000000000000000000, -1.000000000000000000 ) ) ;
#11468 = CARTESIAN_POINT ( 'NONE',  ( -1.999999999999996225, -22.99308372362383679, -14.59552348194486626 ) ) ;
#11469 = CARTESIAN_POINT ( 'NONE',  ( -1.444289557195956863, 16.50319992234354416, 4.262301884875733471 ) ) ;
#11470 = CARTESIAN_POINT ( 'NONE',  ( -3.518350579753606322, 31.87819992234354416, 1.080741659609877781 ) ) ;
#11471 = CARTESIAN_POINT ( 'NONE',  ( -2.481649420246374138, 40.37180007765647360, 0.8687765177876256573 ) ) ;
#11472 = ORIENTED_EDGE ( 'NONE', *, *, #6294, .T. ) ;
#11473 = PRESENTATION_LAYER_ASSIGNMENT (  '', '', ( #14771 ) ) ;
#11474 = CARTESIAN_POINT ( 'NONE',  ( -3.673772985318163098, 34.25319992234354061, 2.599342558261029001 ) ) ;
#11475 = AXIS2_PLACEMENT_3D ( 'NONE', #1584, #11387, #14188 ) ;
#11476 = CIRCLE ( 'NONE', #5573, 2.149999999999995470 ) ;
#11477 = CARTESIAN_POINT ( 'NONE',  ( -4.000000000000004441, -25.33494834008745755, -7.874257998310924656 ) ) ;
#11478 = ORIENTED_EDGE ( 'NONE', *, *, #15984, .T. ) ;
#11479 = DIRECTION ( 'NONE',  ( 0.000000000000000000, 1.000000000000000000, 0.000000000000000000 ) ) ;
#11480 = CARTESIAN_POINT ( 'NONE',  ( -3.481649420246369697, 27.87180007765647360, 1.193696214020542490 ) ) ;
#11481 = CARTESIAN_POINT ( 'NONE',  ( -4.968818199243726141, -10.12411597883879999, -1.720161685108341221 ) ) ;
#11482 = CARTESIAN_POINT ( 'NONE',  ( 4.243569643750003451, -19.64561992126190049, -8.046862975983790633 ) ) ;
#11483 = CARTESIAN_POINT ( 'NONE',  ( 4.481649420246366589, 34.12180007765647360, -1.518615910253458212 ) ) ;
#11484 =( GEOMETRIC_REPRESENTATION_CONTEXT ( 3 ) GLOBAL_UNCERTAINTY_ASSIGNED_CONTEXT ( ( #3806 ) ) GLOBAL_UNIT_ASSIGNED_CONTEXT ( ( #14295, #9004, #13261 ) ) REPRESENTATION_CONTEXT ( 'NONE', 'WORKASPACE' ) );
#11485 = LINE ( 'NONE', #14673, #6475 ) ;
#11486 = ORIENTED_EDGE ( 'NONE', *, *, #2081, .F. ) ;
#11487 = VECTOR ( 'NONE', #13831, 1000.000000000000000 ) ;
#11488 = ORIENTED_EDGE ( 'NONE', *, *, #3605, .F. ) ;
#11489 = CARTESIAN_POINT ( 'NONE',  ( 0.05938372350927906274, 24.87180007765647005, 3.680117784833935701 ) ) ;
#11490 = FACE_OUTER_BOUND ( 'NONE', #10014, .T. ) ;
#11491 = CARTESIAN_POINT ( 'NONE',  ( 10.00000000000000355, 43.00000000000000000, 2.499999999999996891 ) ) ;
#11492 = CARTESIAN_POINT ( 'NONE',  ( -8.500000000000010658, 14.99364916731036956, 20.49999999999998934 ) ) ;
#11493 = EDGE_LOOP ( 'NONE', ( #15205, #82, #3967, #1415, #5952, #17110 ) ) ;
#11494 = CARTESIAN_POINT ( 'NONE',  ( 1.135272562821020070, 17.75319992234354771, -3.311245368580577164 ) ) ;
#11495 = CARTESIAN_POINT ( 'NONE',  ( -1.999999999999996225, -23.57382986613421139, -15.42491492779423723 ) ) ;
#11496 = CARTESIAN_POINT ( 'NONE',  ( 4.243569643749996345, -24.99307287344746342, -7.140837027512114688 ) ) ;
#11497 = CARTESIAN_POINT ( 'NONE',  ( 2.211161402132902243, 39.62180007765646650, 2.942372952327172442 ) ) ;
#11498 = CARTESIAN_POINT ( 'NONE',  ( 0.05938372350920109732, 35.12819992234354771, -3.680117784833935701 ) ) ;
#11499 = CARTESIAN_POINT ( 'NONE',  ( 0.000000000000000000, -2.372474330222551941, 20.89323558166710626 ) ) ;
#11500 = CARTESIAN_POINT ( 'NONE',  ( 0.000000000000000000, 1.759474945355381514, -3.047500000000001652 ) ) ;
#11501 = CIRCLE ( 'NONE', #14207, 4.000000000000000888 ) ;
#11502 = AXIS2_PLACEMENT_3D ( 'NONE', #12768, #7107, #15930 ) ;
#11503 = CARTESIAN_POINT ( 'NONE',  ( 4.730628863548789710E-15, -19.17657787239344458, -11.64849162045545583 ) ) ;
#11504 = CARTESIAN_POINT ( 'NONE',  ( -4.000000000000003553, -2.343145750507612313, 16.84997118393183513 ) ) ;
#11505 = ADVANCED_FACE ( 'NONE', ( #8942 ), #17413, .F. ) ;
#11506 = CARTESIAN_POINT ( 'NONE',  ( -5.679766210340590149, -14.60833734475422752, -5.139172057957636319 ) ) ;
#11507 = EDGE_CURVE ( 'NONE', #6052, #3728, #521, .T. ) ;
#11508 = CARTESIAN_POINT ( 'NONE',  ( 8.499999999999994671, 10.00000000000000000, 22.64999999999999503 ) ) ;
#11509 = AXIS2_PLACEMENT_3D ( 'NONE', #16659, #2741, #6805 ) ;
#11510 = CARTESIAN_POINT ( 'NONE',  ( -1.734723475976807094E-15, 29.79999999999999716, -2.500000000000000000 ) ) ;
#11511 = CARTESIAN_POINT ( 'NONE',  ( -4.243569643749997233, -18.52714587037736393, -6.449516489620252813 ) ) ;
#11512 = EDGE_CURVE ( 'NONE', #15759, #1083, #531, .T. ) ;
#11513 = CARTESIAN_POINT ( 'NONE',  ( -1.158310996484859468, 15.00000000000000533, -3.163418999597361836 ) ) ;
#11514 = DIRECTION ( 'NONE',  ( 3.469446951953612217E-16, -0.000000000000000000, 1.000000000000000000 ) ) ;
#11515 = ORIENTED_EDGE ( 'NONE', *, *, #3073, .F. ) ;
#11516 = AXIS2_PLACEMENT_3D ( 'NONE', #908, #8305, #2758 ) ;
#11517 = CARTESIAN_POINT ( 'NONE',  ( 2.481649420246391902, 18.37819992234354416, 0.8687765177875720335 ) ) ;
#11518 = ADVANCED_FACE ( 'NONE', ( #13022 ), #9110, .T. ) ;
#11519 = CARTESIAN_POINT ( 'NONE',  ( -4.243569643750000786, -26.44909673908217584, -13.49174472062871999 ) ) ;
#11520 = CARTESIAN_POINT ( 'NONE',  ( -2.798362969681365886, 17.74680007765647716, 2.102939460078824929 ) ) ;
#11521 = CARTESIAN_POINT ( 'NONE',  ( 1.336863392178479160, 18.74680007765647005, -4.297206761780677731 ) ) ;
#11522 = DIRECTION ( 'NONE',  ( 0.000000000000000000, 0.8191520442889952403, -0.5735764363510413855 ) ) ;
#11523 = ORIENTED_EDGE ( 'NONE', *, *, #778, .T. ) ;
#11524 = CARTESIAN_POINT ( 'NONE',  ( 4.730628863548789710E-15, -15.82115571973984736, -6.856452161364833486 ) ) ;
#11525 = CARTESIAN_POINT ( 'NONE',  ( -2.211161402132902243, 30.87180007765647716, -2.942372952327172886 ) ) ;
#11526 = CARTESIAN_POINT ( 'NONE',  ( -4.000000000000004441, -21.72141679107589596, -2.713600119290256352 ) ) ;
#11527 = CIRCLE ( 'NONE', #15693, 0.9999999999999991118 ) ;
#11528 = DIRECTION ( 'NONE',  ( 0.000000000000000000, 0.000000000000000000, -1.000000000000000000 ) ) ;
#11529 = CARTESIAN_POINT ( 'NONE',  ( -4.243569643749998122, -23.43122440117877048, -13.45326646829116157 ) ) ;
#11530 = DIRECTION ( 'NONE',  ( 0.000000000000000000, 0.000000000000000000, 1.000000000000000000 ) ) ;
#11531 = DIRECTION ( 'NONE',  ( 0.000000000000000000, 0.000000000000000000, -1.000000000000000000 ) ) ;
#11532 = DIRECTION ( 'NONE',  ( -1.000000000000000000, 0.000000000000000000, 0.000000000000000000 ) ) ;
#11533 = CARTESIAN_POINT ( 'NONE',  ( -4.243569643750000786, -25.41665915365029704, -12.01727104090852905 ) ) ;
#11534 = DIRECTION ( 'NONE',  ( -1.000000000000000000, -0.000000000000000000, -0.000000000000000000 ) ) ;
#11535 = CARTESIAN_POINT ( 'NONE',  ( 1.999999999999994449, -23.44162028740971948, -3.157146360230959292 ) ) ;
#11536 = CARTESIAN_POINT ( 'NONE',  ( -2.481649420246374138, 20.37180007765648426, 0.8687765177876256573 ) ) ;
#11537 = EDGE_CURVE ( 'NONE', #723, #1579, #13249, .T. ) ;
#11538 = ORIENTED_EDGE ( 'NONE', *, *, #842, .F. ) ;
#11539 = CARTESIAN_POINT ( 'NONE',  ( 3.518350579753631191, 24.37180007765647716, 1.080741659609802729 ) ) ;
#11540 = DIRECTION ( 'NONE',  ( -0.000000000000000000, -0.5735764363510414965, -0.8191520442889950182 ) ) ;
#11541 = CARTESIAN_POINT ( 'NONE',  ( 0.000000000000000000, 0.000000000000000000, 0.000000000000000000 ) ) ;
#11542 = CARTESIAN_POINT ( 'NONE',  ( 4.299564228933482956E-15, -19.80093457235270549, -10.97097235620001854 ) ) ;
#11543 = CIRCLE ( 'NONE', #3571, 4.000000000000000000 ) ;
#11544 = CARTESIAN_POINT ( 'NONE',  ( 2.055738996568281518, 35.50319992234354771, -1.423772053676066518 ) ) ;
#11545 = ORIENTED_EDGE ( 'NONE', *, *, #8787, .T. ) ;
#11546 = CARTESIAN_POINT ( 'NONE',  ( -5.330712181944246111E-15, -28.62395502770104017, -8.054784027183542250 ) ) ;
#11547 = CARTESIAN_POINT ( 'NONE',  ( -0.05938372350928957516, 31.12180007765647716, -4.731580009072201776 ) ) ;
#11548 = ORIENTED_EDGE ( 'NONE', *, *, #4884, .T. ) ;
#11549 = DIRECTION ( 'NONE',  ( 0.000000000000000000, 0.000000000000000000, -1.000000000000000000 ) ) ;
#11550 = DIRECTION ( 'NONE',  ( -0.000000000000000000, 1.000000000000000000, -0.000000000000000000 ) ) ;
#11551 = CARTESIAN_POINT ( 'NONE',  ( -4.243569643749997233, -23.46348807572352158, -13.49934377078241710 ) ) ;
#11552 = PLANE ( 'NONE',  #4028 ) ;
#11553 = CIRCLE ( 'NONE', #16627, 6.499999999999999112 ) ;
#11554 = DIRECTION ( 'NONE',  ( -0.000000000000000000, 0.000000000000000000, -1.000000000000000000 ) ) ;
#11555 = FACE_OUTER_BOUND ( 'NONE', #11159, .T. ) ;
#11556 = CARTESIAN_POINT ( 'NONE',  ( 4.730628863548789710E-15, -17.36981209788766378, -9.068162680945119902 ) ) ;
#11557 = ORIENTED_EDGE ( 'NONE', *, *, #9600, .T. ) ;
#11558 = CARTESIAN_POINT ( 'NONE',  ( -8.999999999999996447, -10.00000000000000000, -30.00000000000000000 ) ) ;
#11559 = VERTEX_POINT ( 'NONE', #14524 ) ;
#11560 = ORIENTED_EDGE ( 'NONE', *, *, #3601, .T. ) ;
#11561 = CARTESIAN_POINT ( 'NONE',  ( 3.579096709490575479E-14, -24.93454924669583406, -4.354959555776423130 ) ) ;
#11562 = CARTESIAN_POINT ( 'NONE',  ( 3.604268994871579590, -24.91053875026183562, -15.69445619563776617 ) ) ;
#11563 = CARTESIAN_POINT ( 'NONE',  ( -3.673772985318163098, 21.75319992234354416, 2.599342558261029001 ) ) ;
#11564 = CARTESIAN_POINT ( 'NONE',  ( -1.135272562821019626, 29.00319992234354416, 3.311245368580577164 ) ) ;
#11565 = CARTESIAN_POINT ( 'NONE',  ( 2.481649420246391902, 15.87819992234354771, 0.8687765177875720335 ) ) ;
#11566 = ORIENTED_EDGE ( 'NONE', *, *, #612, .T. ) ;
#11567 = CIRCLE ( 'NONE', #2127, 5.000000000000000000 ) ;
#11568 = CARTESIAN_POINT ( 'NONE',  ( -0.05938372350918959958, 36.37819992234354771, 4.731580009072201776 ) ) ;
#11569 = CARTESIAN_POINT ( 'NONE',  ( -3.999999999999997335, -21.85257474295189084, -10.95354890098744605 ) ) ;
#11570 = ORIENTED_EDGE ( 'NONE', *, *, #8861, .T. ) ;
#11571 = EDGE_CURVE ( 'NONE', #9180, #4032, #9978, .T. ) ;
#11572 = CARTESIAN_POINT ( 'NONE',  ( 8.500000000000001776, 13.00000000000000000, -20.49999999999999645 ) ) ;
#11573 = EDGE_CURVE ( 'NONE', #16267, #17729, #1432, .T. ) ;
#11574 = CARTESIAN_POINT ( 'NONE',  ( 1.027846397803542144, 33.74680007765648071, -3.346150245485522312 ) ) ;
#11575 = CARTESIAN_POINT ( 'NONE',  ( -5.348698796015789014, -10.20673381021435411, -1.142656398237904991 ) ) ;
#11576 = EDGE_CURVE ( 'NONE', #9180, #7134, #5975, .T. ) ;
#11577 = CARTESIAN_POINT ( 'NONE',  ( 4.243569643750000786, -22.19029169917569888, -7.409540791782929681 ) ) ;
#11578 = CARTESIAN_POINT ( 'NONE',  ( -4.499999999999999112, 32.99680007765648071, 0.05647727720537927543 ) ) ;
#11579 = EDGE_CURVE ( 'NONE', #1682, #6052, #1727, .T. ) ;
#11580 = DIRECTION ( 'NONE',  ( 0.000000000000000000, -0.5000000000000012212, -0.8660254037844380415 ) ) ;
#11581 = ORIENTED_EDGE ( 'NONE', *, *, #15525, .T. ) ;
#11582 = ORIENTED_EDGE ( 'NONE', *, *, #9219, .F. ) ;
#11583 = CARTESIAN_POINT ( 'NONE',  ( -3.518350579753630747, 20.62180007765646650, -1.080741659609802729 ) ) ;
#11584 = CARTESIAN_POINT ( 'NONE',  ( -1.734723475976807094E-15, 16.59999999999999787, -10.50000000000000178 ) ) ;
#11585 = CARTESIAN_POINT ( 'NONE',  ( -1.071796769724496334, -29.33393568550013342, -10.63793452924315375 ) ) ;
#11586 = CARTESIAN_POINT ( 'NONE',  ( 0.000000000000000000, -10.00099999999999767, 0.000000000000000000 ) ) ;
#11587 = CARTESIAN_POINT ( 'NONE',  ( -4.648177544792955347E-16, -29.77410042770280185, -11.26655492845805107 ) ) ;
#11588 = ORIENTED_EDGE ( 'NONE', *, *, #11344, .T. ) ;
#11589 = CARTESIAN_POINT ( 'NONE',  ( 0.05938372350920109732, 22.62819992234354416, -3.680117784833935701 ) ) ;
#11590 = LINE ( 'NONE', #7421, #15777 ) ;
#11591 = CARTESIAN_POINT ( 'NONE',  ( -5.330712181944245322E-15, -26.78492557865051538, -5.428377785181952575 ) ) ;
#11592 = CARTESIAN_POINT ( 'NONE',  ( -0.05938372350927861171, 38.62180007765648071, -3.680117784833935701 ) ) ;
#11593 = CIRCLE ( 'NONE', #16958, 0.9999999999999991118 ) ;
#11594 = CARTESIAN_POINT ( 'NONE',  ( 1.135272562821020070, 32.75319992234354771, -3.311245368580577164 ) ) ;
#11595 = AXIS2_PLACEMENT_3D ( 'NONE', #17281, #14678, #4552 ) ;
#11596 = CARTESIAN_POINT ( 'NONE',  ( 4.243569643750000786, -27.12663390452184942, -14.45936807294509308 ) ) ;
#11597 = CARTESIAN_POINT ( 'NONE',  ( 2.000000000000004441, -24.32664893814001417, -16.50005198491677305 ) ) ;
#11598 = AXIS2_PLACEMENT_3D ( 'NONE', #1933, #15919, #1639 ) ;
#11599 = CARTESIAN_POINT ( 'NONE',  ( 4.243569643749996345, -25.02533654799221097, -7.186914330003371099 ) ) ;
#11600 = CARTESIAN_POINT ( 'NONE',  ( 10.00000000000000000, 16.59999999999999787, -2.500000000000003109 ) ) ;
#11601 = AXIS2_PLACEMENT_3D ( 'NONE', #11126, #18213, #5481 ) ;
#11602 = CARTESIAN_POINT ( 'NONE',  ( -4.757769075324985941, -14.90261145393141895, -7.125238870421979342 ) ) ;
#11603 = AXIS2_PLACEMENT_3D ( 'NONE', #554, #14841, #6290 ) ;
#11604 = DIRECTION ( 'NONE',  ( 0.000000000000000000, 0.000000000000000000, 1.000000000000000000 ) ) ;
#11605 = AXIS2_PLACEMENT_3D ( 'NONE', #1394, #15572, #2871 ) ;
#11606 = DIRECTION ( 'NONE',  ( 0.000000000000000000, -0.5735764363510414965, -0.8191520442889950182 ) ) ;
#11607 = ORIENTED_EDGE ( 'NONE', *, *, #9214, .F. ) ;
#11608 = CARTESIAN_POINT ( 'NONE',  ( -4.243569643750005227, -22.49801537532042062, -3.577525634854993086 ) ) ;
#11609 = CARTESIAN_POINT ( 'NONE',  ( 8.499999999999994671, 15.00000000000000178, 20.49999999999999645 ) ) ;
#11610 = DIRECTION ( 'NONE',  ( 1.000000000000000000, 0.000000000000000000, -4.336808689942021680E-16 ) ) ;
#11611 = VERTEX_POINT ( 'NONE', #8846 ) ;
#11612 = CARTESIAN_POINT ( 'NONE',  ( 1.593127413382953383, 20.37819992234354771, -2.091722143975172532 ) ) ;
#11613 = CARTESIAN_POINT ( 'NONE',  ( 0.000000000000000000, 15.00000000000000355, 0.000000000000000000 ) ) ;
#11614 = DIRECTION ( 'NONE',  ( 0.000000000000000000, 0.000000000000000000, 1.000000000000000000 ) ) ;
#11615 = CARTESIAN_POINT ( 'NONE',  ( 0.3999999999999975797, 0.000000000000000000, 0.000000000000000000 ) ) ;
#11616 = CARTESIAN_POINT ( 'NONE',  ( 3.049298716198209913, -9.999999999999397815, -3.862741893372411806 ) ) ;
#11617 = EDGE_LOOP ( 'NONE', ( #4970, #7418, #14840 ) ) ;
#11618 = AXIS2_PLACEMENT_3D ( 'NONE', #13975, #17993, #14060 ) ;
#11619 = CARTESIAN_POINT ( 'NONE',  ( -3.518350579753630747, 38.12180007765648071, -1.080741659609802729 ) ) ;
#11620 = AXIS2_PLACEMENT_3D ( 'NONE', #15871, #3075, #7139 ) ;
#11621 = CARTESIAN_POINT ( 'NONE',  ( -4.243569643750000786, -26.22325101726895369, -13.16920360318992955 ) ) ;
#11622 = CARTESIAN_POINT ( 'NONE',  ( -4.000000000000004441, -26.94813206802970740, -10.17812312388048746 ) ) ;
#11623 = CARTESIAN_POINT ( 'NONE',  ( 4.243569643750003451, -23.51726086663143533, -13.57613927493450667 ) ) ;
#11624 = CARTESIAN_POINT ( 'NONE',  ( 8.000000000000000000, 40.79999999999999716, -2.500000000000000888 ) ) ;
#11625 = EDGE_CURVE ( 'NONE', #6401, #4895, #5260, .T. ) ;
#11626 = CARTESIAN_POINT ( 'NONE',  ( 14.20000000000000107, 0.000000000000000000, 0.000000000000000000 ) ) ;
#11627 = FACE_OUTER_BOUND ( 'NONE', #1940, .T. ) ;
#11628 = CARTESIAN_POINT ( 'NONE',  ( -4.243569643750005227, -27.40209390612182716, -10.58127561352589829 ) ) ;
#11629 = CARTESIAN_POINT ( 'NONE',  ( 4.000000000000000888, -21.85152311680833748, -6.925729116128124474 ) ) ;
#11630 = CARTESIAN_POINT ( 'NONE',  ( -2.000000000000005773, -22.96841972742010540, -2.481345923692543920 ) ) ;
#11631 = TOROIDAL_SURFACE ( 'NONE', #7153, 9.000000000000003553, 0.9999999999999991118 ) ;
#11632 = CARTESIAN_POINT ( 'NONE',  ( 2.500000000000001332, 24.24680007765647716, -0.05647727720535888202 ) ) ;
#11633 = VERTEX_POINT ( 'NONE', #11815 ) ;
#11634 = CARTESIAN_POINT ( 'NONE',  ( -2.864755990943265829, 20.74680007765647716, -2.011557305968488141 ) ) ;
#11635 = CYLINDRICAL_SURFACE ( 'NONE', #9247, 2.499999999999999556 ) ;
#11636 = DIRECTION ( 'NONE',  ( 0.000000000000000000, -1.000000000000000000, 0.000000000000000000 ) ) ;
#11637 = CARTESIAN_POINT ( 'NONE',  ( -1.734723475976807094E-15, 29.79999999999999716, -2.500000000000000000 ) ) ;
#11638 = CARTESIAN_POINT ( 'NONE',  ( 2.211161402132839626, 15.37819992234354771, -2.942372952327218183 ) ) ;
#11639 = ORIENTED_EDGE ( 'NONE', *, *, #7933, .T. ) ;
#11640 = CARTESIAN_POINT ( 'NONE',  ( -2.121784821875005722, -27.38388281328888141, -8.419522421775232246 ) ) ;
#11641 = CARTESIAN_POINT ( 'NONE',  ( -4.518350579753632523, 38.12180007765647360, -1.405661355842698468 ) ) ;
#11642 = ORIENTED_EDGE ( 'NONE', *, *, #7961, .T. ) ;
#11643 = AXIS2_PLACEMENT_3D ( 'NONE', #14609, #510, #6153 ) ;
#11644 = CARTESIAN_POINT ( 'NONE',  ( 2.000000000000004441, -18.64824221826470207, -8.390446746455726412 ) ) ;
#11645 = ADVANCED_FACE ( 'NONE', ( #11627 ), #6737, .F. ) ;
#11646 = LINE ( 'NONE', #14443, #15090 ) ;
#11647 = AXIS2_PLACEMENT_3D ( 'NONE', #14616, #424, #17409 ) ;
#11648 = CARTESIAN_POINT ( 'NONE',  ( -5.330712181944245322E-15, -30.17261140584885126, -10.26649454676382867 ) ) ;
#11649 = CARTESIAN_POINT ( 'NONE',  ( 1.300000000000000044, 0.7216878364870329410, -1.250000000000000000 ) ) ;
#11650 = FACE_OUTER_BOUND ( 'NONE', #6978, .T. ) ;
#11651 = CARTESIAN_POINT ( 'NONE',  ( 4.000000000000000888, -23.65828889131411827, -9.506058055638460402 ) ) ;
#11652 = AXIS2_PLACEMENT_3D ( 'NONE', #10560, #6113, #2058 ) ;
#11653 = CARTESIAN_POINT ( 'NONE',  ( 2.121784821875004390, -17.87857435595223876, -7.659005429884962801 ) ) ;
#11654 = ORIENTED_EDGE ( 'NONE', *, *, #818, .F. ) ;
#11655 = CARTESIAN_POINT ( 'NONE',  ( 8.499999999999994671, 10.00000000000000000, 20.49999999999999645 ) ) ;
#11656 = CARTESIAN_POINT ( 'NONE',  ( 4.000000000000000000, -3.004629197474318457E-15, -3.047499999999999876 ) ) ;
#11657 = ORIENTED_EDGE ( 'NONE', *, *, #483, .F. ) ;
#11658 = VERTEX_POINT ( 'NONE', #10233 ) ;
#11659 = CARTESIAN_POINT ( 'NONE',  ( 0.000000000000000000, 5.000000000000000000, 0.000000000000000000 ) ) ;
#11660 = DIRECTION ( 'NONE',  ( 0.000000000000000000, -0.000000000000000000, 1.000000000000000000 ) ) ;
#11661 = SHAPE_REPRESENTATION_RELATIONSHIP ( 'NONE' , 'NONE' ,  #5306, #7836 ) ;
#11662 = CARTESIAN_POINT ( 'NONE',  ( 0.05938372350919016857, 27.62819992234354416, -4.731580009072201776 ) ) ;
#11663 = CARTESIAN_POINT ( 'NONE',  ( 3.518350579753606322, 28.12819992234354416, -1.080741659609876892 ) ) ;
#11664 = CARTESIAN_POINT ( 'NONE',  ( 0.7188294034286553114, 16.25319992234354771, 2.395093729190349130 ) ) ;
#11665 = EDGE_LOOP ( 'NONE', ( #7838, #866 ) ) ;
#11666 = CARTESIAN_POINT ( 'NONE',  ( -1.444289557195956863, 34.00319992234354771, 4.262301884875733471 ) ) ;
#11667 = CARTESIAN_POINT ( 'NONE',  ( 2.000000000000004441, -19.42257040733860762, -9.496302006245869620 ) ) ;
#11668 = VERTEX_POINT ( 'NONE', #3395 ) ;
#11669 = DIRECTION ( 'NONE',  ( 0.000000000000000000, 0.000000000000000000, 1.000000000000000000 ) ) ;
#11670 = CARTESIAN_POINT ( 'NONE',  ( -1.027846397803541700, 32.49680007765648071, 3.346150245485522312 ) ) ;
#11671 = CARTESIAN_POINT ( 'NONE',  ( -7.496931198983602052, -13.00340931249926157, 5.026614306467389603 ) ) ;
#11672 = CARTESIAN_POINT ( 'NONE',  ( -4.243569643750000786, -21.54501820828076930, -6.487994741957813005 ) ) ;
#11673 = CARTESIAN_POINT ( 'NONE',  ( 3.607379964056306676, 31.49680007765647716, -2.690724712371305838 ) ) ;
#11674 = DIRECTION ( 'NONE',  ( 0.000000000000000000, 0.000000000000000000, -1.000000000000000000 ) ) ;
#11675 = ORIENTED_EDGE ( 'NONE', *, *, #201, .T. ) ;
#11676 = CARTESIAN_POINT ( 'NONE',  ( 1.135272562821090458, 32.24680007765648071, 3.311245368580554072 ) ) ;
#11677 = CARTESIAN_POINT ( 'NONE',  ( -1.071796769724486786, -19.98298991819740422, -11.23097433548487700 ) ) ;
#11678 = ADVANCED_FACE ( 'NONE', ( #9037 ), #7639, .T. ) ;
#11679 = CARTESIAN_POINT ( 'NONE',  ( -8.999999999999996447, -10.00000000000000000, 15.14468620625656925 ) ) ;
#11680 = CARTESIAN_POINT ( 'NONE',  ( -4.000000000000000888, -26.56201959963631509, -13.65301527884473387 ) ) ;
#11681 = ORIENTED_EDGE ( 'NONE', *, *, #17049, .F. ) ;
#11682 = CARTESIAN_POINT ( 'NONE',  ( -2.864755990943222308, 29.25319992234354416, 2.011557305968548093 ) ) ;
#11683 = EDGE_CURVE ( 'NONE', #1143, #1567, #7324, .T. ) ;
#11684 = DIRECTION ( 'NONE',  ( 0.000000000000000000, 0.5000000000000012212, 0.8660254037844380415 ) ) ;
#11685 = CARTESIAN_POINT ( 'NONE',  ( 4.243569643749996345, -22.92819770258371292, -4.191889668071731911 ) ) ;
#11686 = CARTESIAN_POINT ( 'NONE',  ( -1.135272562821090014, 38.49680007765647360, -3.311245368580554072 ) ) ;
#11687 =( BOUNDED_CURVE ( )  B_SPLINE_CURVE ( 2, ( #12584, #3882, #5456, #16609, #8324, #2599, #15393, #11278, #7009 ),
 .UNSPECIFIED., .F., .F. ) 
 B_SPLINE_CURVE_WITH_KNOTS ( ( 3, 2, 2, 2, 3 ),
 ( 0.3879310344827586188, 0.3908045977011494476, 0.3965517241379310498, 0.4022988505747126520, 0.4051724137931034808 ),
 .UNSPECIFIED. ) 
 CURVE ( )  GEOMETRIC_REPRESENTATION_ITEM ( )  RATIONAL_B_SPLINE_CURVE ( ( 0.9330127018922194093, 0.9330127018922194093, 1.000000000000000000, 0.8660254037844387076, 1.000000000000000000, 0.8660254037844387076, 1.000000000000000000, 0.9330127018922187432, 0.9330127018922194093 ) ) 
 REPRESENTATION_ITEM ( '' )  );
#11688 = CARTESIAN_POINT ( 'NONE',  ( 2.211161402132839626, 37.87819992234352640, -2.942372952327218183 ) ) ;
#11689 = CARTESIAN_POINT ( 'NONE',  ( -4.243569643749998122, -25.01214445387132912, -15.71105429036270351 ) ) ;
#11690 = CARTESIAN_POINT ( 'NONE',  ( 3.999999999999996447, -28.60433402728840946, -12.54342465075819035 ) ) ;
#11691 = EDGE_CURVE ( 'NONE', #8670, #12774, #15625, .T. ) ;
#11692 = CARTESIAN_POINT ( 'NONE',  ( -4.243569643749997233, -20.10806592306992613, -8.707304311691796528 ) ) ;
#11693 = CARTESIAN_POINT ( 'NONE',  ( -10.00000000000000000, 36.39999999999999147, 2.499999999999998224 ) ) ;
#11694 = DIRECTION ( 'NONE',  ( -0.000000000000000000, 1.000000000000000000, -0.000000000000000000 ) ) ;
#11695 = PLANE ( 'NONE',  #309 ) ;
#11696 = CARTESIAN_POINT ( 'NONE',  ( -2.000000000000005773, -27.54986151206910350, -9.024322876444124120 ) ) ;
#11697 = ORIENTED_EDGE ( 'NONE', *, *, #5157, .T. ) ;
#11698 = ORIENTED_EDGE ( 'NONE', *, *, #14417, .T. ) ;
#11699 = CARTESIAN_POINT ( 'NONE',  ( -5.330712181944245322E-15, -23.68761282235488963, -1.004956746021377967 ) ) ;
#11700 = DIRECTION ( 'NONE',  ( 0.000000000000000000, 0.000000000000000000, 1.000000000000000000 ) ) ;
#11701 = ORIENTED_EDGE ( 'NONE', *, *, #13795, .F. ) ;
#11702 = CARTESIAN_POINT ( 'NONE',  ( -1.593127413382952939, 16.62819992234354061, 2.091722143975172532 ) ) ;
#11703 = ADVANCED_FACE ( 'NONE', ( #17869 ), #16377, .F. ) ;
#11704 = CARTESIAN_POINT ( 'NONE',  ( -2.121784821875005722, -28.38405672417600911, -9.847918799004165891 ) ) ;
#11705 = DIRECTION ( 'NONE',  ( 1.049727191973305394E-16, 0.5150380737757255245, -0.8571673013836856869 ) ) ;
#11706 = AXIS2_PLACEMENT_3D ( 'NONE', #11499, #9011, #11782 ) ;
#11707 = CARTESIAN_POINT ( 'NONE',  ( -8.000000000000000000, 13.00000000000000178, 2.500000000000000000 ) ) ;
#11708 = VECTOR ( 'NONE', #1753, 1000.000000000000114 ) ;
#11709 = CARTESIAN_POINT ( 'NONE',  ( 7.003832385457680054, -10.00000000000000178, -7.945690313593527954 ) ) ;
#11710 = EDGE_LOOP ( 'NONE', ( #8080, #5818, #3411 ) ) ;
#11711 = CARTESIAN_POINT ( 'NONE',  ( -3.500000000000000444, 37.99680007765647360, 0.05647727720536892260 ) ) ;
#11712 = CARTESIAN_POINT ( 'NONE',  ( 4.730628863548789710E-15, -22.27389062868906677, -16.07191265961602511 ) ) ;
#11713 = DIRECTION ( 'NONE',  ( -0.000000000000000000, -1.000000000000000000, -0.000000000000000000 ) ) ;
#11714 = CARTESIAN_POINT ( 'NONE',  ( -2.121784821874996396, -22.96548037584052793, -14.92386012267298945 ) ) ;
#11715 = VECTOR ( 'NONE', #2904, 1000.000000000000000 ) ;
#11716 = CYLINDRICAL_SURFACE ( 'NONE', #5810, 4.000000000000000000 ) ;
#11717 = CARTESIAN_POINT ( 'NONE',  ( -8.000000000000003553, 43.00000000000000000, -2.500000000000001776 ) ) ;
#11718 = CARTESIAN_POINT ( 'NONE',  ( 3.579096709490575479E-14, -24.61191250054342916, -3.894186529857098567 ) ) ;
#11719 = AXIS2_PLACEMENT_3D ( 'NONE', #8747, #4676, #10325 ) ;
#11720 = CARTESIAN_POINT ( 'NONE',  ( -4.243569643750000786, -23.86800277550248950, -9.805560521328242629 ) ) ;
#11721 = CARTESIAN_POINT ( 'NONE',  ( -3.500000000000000444, 14.50319992234354416, -0.05647727720529563400 ) ) ;
#11722 = DIRECTION ( 'NONE',  ( -0.000000000000000000, -1.000000000000000000, -0.000000000000000000 ) ) ;
#11723 = CARTESIAN_POINT ( 'NONE',  ( 1.989345975306426206, 26.49680007765648426, -1.515154207786343799 ) ) ;
#11724 = ORIENTED_EDGE ( 'NONE', *, *, #9701, .T. ) ;
#11725 = CARTESIAN_POINT ( 'NONE',  ( 2.864755990943265829, 19.49680007765648071, 2.011557305968487697 ) ) ;
#11726 = CARTESIAN_POINT ( 'NONE',  ( 8.500000000000019540, 0.000000000000000000, 18.49999999999998934 ) ) ;
#11727 = CARTESIAN_POINT ( 'NONE',  ( -4.000000000000004441, -27.46435086074563969, -10.91535996374058293 ) ) ;
#11728 = CARTESIAN_POINT ( 'NONE',  ( 2.000000000000004441, -17.42222258626929943, -6.639509252794765892 ) ) ;
#11729 = CARTESIAN_POINT ( 'NONE',  ( 1.135272562821020070, 22.75319992234354416, -3.311245368580577164 ) ) ;
#11730 = EDGE_LOOP ( 'NONE', ( #7579, #349 ) ) ;
#11731 = CARTESIAN_POINT ( 'NONE',  ( 4.730628863548789710E-15, -20.20901545782531628, -13.12296530017564500 ) ) ;
#11732 = CARTESIAN_POINT ( 'NONE',  ( 1.336863392178479160, 38.74680007765646650, -4.297206761780677731 ) ) ;
#11733 = AXIS2_PLACEMENT_3D ( 'NONE', #4583, #14711, #12922 ) ;
#11734 = ORIENTED_EDGE ( 'NONE', *, *, #2712, .T. ) ;
#11735 = FACE_OUTER_BOUND ( 'NONE', #13316, .T. ) ;
#11736 = CARTESIAN_POINT ( 'NONE',  ( 4.000000000000000888, -20.04475734230255668, -4.345400176617791210 ) ) ;
#11737 = CARTESIAN_POINT ( 'NONE',  ( 4.243569643750000786, -25.83608692273200802, -12.61627597329485440 ) ) ;
#11738 = CARTESIAN_POINT ( 'NONE',  ( -4.000000000000004441, -27.20624146438767710, -10.54674154381053697 ) ) ;
#11739 = CARTESIAN_POINT ( 'NONE',  ( 4.000000000000000000, 2.639212418033077601, 1.523749999999997717 ) ) ;
#11740 = CARTESIAN_POINT ( 'NONE',  ( 4.243569643750000786, -21.19011778828857118, -5.981144414553994260 ) ) ;
#11741 = ORIENTED_EDGE ( 'NONE', *, *, #506, .T. ) ;
#11742 = CARTESIAN_POINT ( 'NONE',  ( 2.610817454768295409, -22.11373505648317916, -1.875566028523329321 ) ) ;
#11743 = EDGE_CURVE ( 'NONE', #3783, #1108, #17785, .T. ) ;
#11744 = CARTESIAN_POINT ( 'NONE',  ( 4.299564228933482956E-15, -19.99451661891623289, -11.24743617014079078 ) ) ;
#11745 = LINE ( 'NONE', #1759, #7615 ) ;
#11746 = ORIENTED_EDGE ( 'NONE', *, *, #8620, .F. ) ;
#11747 = AXIS2_PLACEMENT_3D ( 'NONE', #704, #6351, #7821 ) ;
#11748 = ORIENTED_EDGE ( 'NONE', *, *, #10859, .T. ) ;
#11749 = CARTESIAN_POINT ( 'NONE',  ( 3.999999999999996447, -26.08776741350315831, -8.949395057446990265 ) ) ;
#11750 = ADVANCED_FACE ( 'NONE', ( #3933, #12087, #3665 ), #16463, .F. ) ;
#11751 = DIRECTION ( 'NONE',  ( -3.469446951953613696E-16, -0.000000000000000000, -1.000000000000000000 ) ) ;
#11752 =( NAMED_UNIT ( * ) SI_UNIT ( $, .STERADIAN. ) SOLID_ANGLE_UNIT ( ) );
#11753 = CARTESIAN_POINT ( 'NONE',  ( -2.733110507866328476, 24.87819992234354771, -3.862833514489096398 ) ) ;
#11754 = CARTESIAN_POINT ( 'NONE',  ( 2.115076519116425580, 38.62819992234354061, 3.012182706137062294 ) ) ;
#11755 = EDGE_CURVE ( 'NONE', #9470, #1591, #5136, .T. ) ;
#11756 = CARTESIAN_POINT ( 'NONE',  ( -0.8262555684460826111, 19.00319992234354771, 2.360188852285421302 ) ) ;
#11757 = ORIENTED_EDGE ( 'NONE', *, *, #12450, .F. ) ;
#11758 = CARTESIAN_POINT ( 'NONE',  ( 2.733110507866247652, 18.87180007765647716, -3.862833514489153686 ) ) ;
#11759 = CARTESIAN_POINT ( 'NONE',  ( -4.000000000000000888, -21.65794106883490855, -6.649265300173826887 ) ) ;
#11760 = VERTEX_POINT ( 'NONE', #7914 ) ;
#11761 = LINE ( 'NONE', #4906, #11814 ) ;
#11762 = CIRCLE ( 'NONE', #8495, 10.00000000000000000 ) ;
#11763 = CARTESIAN_POINT ( 'NONE',  ( 2.864755990943265829, 26.99680007765648071, 2.011557305968487697 ) ) ;
#11764 = DIRECTION ( 'NONE',  ( -0.7071067811865383579, 8.659560562355047490E-17, -0.7071067811865567876 ) ) ;
#11765 = CARTESIAN_POINT ( 'NONE',  ( 4.243569643749997233, -23.18630709894168263, -4.560508088001781424 ) ) ;
#11766 = CARTESIAN_POINT ( 'NONE',  ( -3.607379964056306676, 30.24680007765647360, 2.690724712371306282 ) ) ;
#11767 = CARTESIAN_POINT ( 'NONE',  ( 3.999999999999996447, -21.89348972198121857, -2.959345732576948773 ) ) ;
#11768 = ORIENTED_EDGE ( 'NONE', *, *, #11119, .F. ) ;
#11769 = CARTESIAN_POINT ( 'NONE',  ( 2.864755990943265829, 31.99680007765647716, 2.011557305968487697 ) ) ;
#11770 = CARTESIAN_POINT ( 'NONE',  ( 14.99999999999999822, 10.00000000000000000, -25.00000000000000355 ) ) ;
#11771 = CARTESIAN_POINT ( 'NONE',  ( 9.000000000000005329, 43.00000000000000000, 2.499999999999997335 ) ) ;
#11772 = CYLINDRICAL_SURFACE ( 'NONE', #8632, 4.000000000000000000 ) ;
#11773 = DIRECTION ( 'NONE',  ( -0.000000000000000000, -1.000000000000000000, -0.000000000000000000 ) ) ;
#11774 = VERTEX_POINT ( 'NONE', #15164 ) ;
#11775 = CIRCLE ( 'NONE', #8508, 2.000000000000001776 ) ;
#11776 = CARTESIAN_POINT ( 'NONE',  ( 2.864755990943222308, 30.50319992234354416, -2.011557305968548093 ) ) ;
#11777 = DIRECTION ( 'NONE',  ( 0.000000000000000000, 0.000000000000000000, 1.000000000000000000 ) ) ;
#11778 = AXIS2_PLACEMENT_3D ( 'NONE', #14713, #335, #10138 ) ;
#11779 = CARTESIAN_POINT ( 'NONE',  ( -4.243569643750005227, -24.04667175346823527, -5.789236154435278614 ) ) ;
#11780 = CARTESIAN_POINT ( 'NONE',  ( 2.481649420246374138, 24.12180007765648071, -0.8687765177876252132 ) ) ;
#11781 = CARTESIAN_POINT ( 'NONE',  ( -0.05938372350918959958, 18.87819992234354416, 4.731580009072201776 ) ) ;
#11782 = DIRECTION ( 'NONE',  ( 0.000000000000000000, 0.8191520442889952403, -0.5735764363510411634 ) ) ;
#11783 = CARTESIAN_POINT ( 'NONE',  ( -5.279047395330986450E-15, -30.02288408040872625, -10.54300617450737043 ) ) ;
#11784 = CARTESIAN_POINT ( 'NONE',  ( -4.243569643750000786, -21.57728188282551685, -6.534072044449069416 ) ) ;
#11785 = LINE ( 'NONE', #14395, #11881 ) ;
#11786 = PRESENTATION_LAYER_ASSIGNMENT (  '', '', ( #5592 ) ) ;
#11787 = EDGE_CURVE ( 'NONE', #15972, #6854, #8510, .T. ) ;
#11788 = CARTESIAN_POINT ( 'NONE',  ( -8.999999999999996447, -10.00000000000000178, -3.713574246709370641 ) ) ;
#11789 = CARTESIAN_POINT ( 'NONE',  ( 1.071796769724494114, -23.61957486864662314, -16.42455588381737286 ) ) ;
#11790 = DIRECTION ( 'NONE',  ( 0.000000000000000000, 0.000000000000000000, -1.000000000000000000 ) ) ;
#11791 = EDGE_LOOP ( 'NONE', ( #16143, #1439, #3464, #11285 ) ) ;
#11792 = ORIENTED_EDGE ( 'NONE', *, *, #12042, .T. ) ;
#11793 =( BOUNDED_CURVE ( )  B_SPLINE_CURVE ( 2, ( #9309, #3744, #3664, #13479, #13304, #9395, #14902, #792, #14983 ),
 .UNSPECIFIED., .F., .F. ) 
 B_SPLINE_CURVE_WITH_KNOTS ( ( 3, 2, 2, 2, 3 ),
 ( 0.1120689655172413812, 0.1149425287356321823, 0.1206896551724137984, 0.1264367816091954144, 0.1293103448275862155 ),
 .UNSPECIFIED. ) 
 CURVE ( )  GEOMETRIC_REPRESENTATION_ITEM ( )  RATIONAL_B_SPLINE_CURVE ( ( 0.9330127018922194093, 0.9330127018922194093, 1.000000000000000000, 0.8660254037844387076, 1.000000000000000000, 0.8660254037844387076, 1.000000000000000000, 0.9330127018922194093, 0.9330127018922194093 ) ) 
 REPRESENTATION_ITEM ( '' )  );
#11794 = DIRECTION ( 'NONE',  ( -0.7071067811865383579, 0.000000000000000000, 0.7071067811865567876 ) ) ;
#11795 = CARTESIAN_POINT ( 'NONE',  ( -1.734723475976807094E-15, 18.79999999999999361, -10.50000000000000178 ) ) ;
#11796 = DIRECTION ( 'NONE',  ( 0.000000000000000000, 1.000000000000000000, 0.000000000000000000 ) ) ;
#11797 = EDGE_LOOP ( 'NONE', ( #15557, #14694, #4362, #14403 ) ) ;
#11798 = CARTESIAN_POINT ( 'NONE',  ( -2.481649420246391902, 27.12819992234355126, -0.8687765177875723666 ) ) ;
#11799 = CARTESIAN_POINT ( 'NONE',  ( 4.243569643750003451, -23.51726086663143533, -13.57613927493450667 ) ) ;
#11800 = CARTESIAN_POINT ( 'NONE',  ( 3.500000000000000444, 19.24680007765648071, -0.05647727720536935281 ) ) ;
#11801 = CIRCLE ( 'NONE', #573, 0.9999999999999991118 ) ;
#11802 = DIRECTION ( 'NONE',  ( 0.000000000000000000, 0.000000000000000000, -1.000000000000000000 ) ) ;
#11803 = DIRECTION ( 'NONE',  ( -0.000000000000000000, -0.5735764363510414965, -0.8191520442889950182 ) ) ;
#11804 = ORIENTED_EDGE ( 'NONE', *, *, #13450, .T. ) ;
#11805 = CARTESIAN_POINT ( 'NONE',  ( -2.115076519116362519, 37.62180007765648071, 3.012182706137107147 ) ) ;
#11806 = CARTESIAN_POINT ( 'NONE',  ( -2.121784821875005722, -28.67442979507872636, -10.26261452142547093 ) ) ;
#11807 = EDGE_CURVE ( 'NONE', #8124, #4416, #10591, .T. ) ;
#11808 = SURFACE_STYLE_USAGE ( .BOTH. , #6160 ) ;
#11809 = EDGE_CURVE ( 'NONE', #3185, #5643, #13850, .T. ) ;
#11810 = CARTESIAN_POINT ( 'NONE',  ( 4.243569643750000786, -23.99705747368147968, -9.989869731293264721 ) ) ;
#11811 = DIRECTION ( 'NONE',  ( -0.000000000000000000, -0.000000000000000000, -1.000000000000000000 ) ) ;
#11812 = CIRCLE ( 'NONE', #15480, 7.000000000000000000 ) ;
#11813 = CARTESIAN_POINT ( 'NONE',  ( -8.500000000000005329, 0.000000000000000000, -18.49999999999999645 ) ) ;
#11814 = VECTOR ( 'NONE', #10557, 1000.000000000000000 ) ;
#11815 = CARTESIAN_POINT ( 'NONE',  ( -8.500000000000005329, -1.201721234452885367, -20.49999999999999645 ) ) ;
#11816 = CARTESIAN_POINT ( 'NONE',  ( 2.121784821875004390, -20.42740464498717401, -11.29911232669418197 ) ) ;
#11817 = CARTESIAN_POINT ( 'NONE',  ( 1.999999999999994449, -24.73216726919956443, -5.000238459881198416 ) ) ;
#11818 = DIRECTION ( 'NONE',  ( 1.000000000000000000, 0.000000000000000000, -4.336808689942021680E-16 ) ) ;
#11819 = CARTESIAN_POINT ( 'NONE',  ( 2.055738996568313048, 34.49680007765648071, 1.423772053676023441 ) ) ;
#11820 = ORIENTED_EDGE ( 'NONE', *, *, #14908, .T. ) ;
#11821 = CARTESIAN_POINT ( 'NONE',  ( -2.211161402132901799, 18.37180007765647716, -2.942372952327172886 ) ) ;
#11822 = DIRECTION ( 'NONE',  ( 0.000000000000000000, 0.000000000000000000, -1.000000000000000000 ) ) ;
#11823 =( LENGTH_UNIT ( ) NAMED_UNIT ( * ) SI_UNIT ( .MILLI., .METRE. ) );
#11824 = CARTESIAN_POINT ( 'NONE',  ( -4.000000000000004441, -27.20624146438767355, -10.54674154381053697 ) ) ;
#11825 = VECTOR ( 'NONE', #14314, 1000.000000000000000 ) ;
#11826 = CARTESIAN_POINT ( 'NONE',  ( 4.299564228933482956E-15, -17.92964144805248594, -8.298488810700408891 ) ) ;
#11827 = CARTESIAN_POINT ( 'NONE',  ( -2.211161402132839182, 16.62819992234354416, 2.942372952327218627 ) ) ;
#11828 =( BOUNDED_SURFACE ( )  B_SPLINE_SURFACE ( 1, 2, ( 
 ( #7164, #12824, #16938, #15804, #3006, #10217, #3100, #17028, #15616, #8641, #320, #15897, #14319, #9945, #8461, #8732, #14406, #7071, #14511, #1617, #7250, #2917, #1529, #220, #12910, #18332, #5869, #8832, #14129, #13007, #11519, #17209, #6981, #1712, #4211, #9858, #2830, #4298, #16365, #604, #3651, #3566, #508, #14606, #10692, #9298, #16273, #2000, #4944, #11894, #17593, #13291, #5036, #9212, #10313, #12075, #6244, #1808, #2093, #6343, #17774, #8925, #4856, #1908, #10507, #17680, #7538, #14890, #13382, #7444, #16176, #6150, #13191, #11799, #13102, #17496, #416, #17399, #13472, #6054, #11704, #4761, #2187, #4663, #3473, #15996, #9117, #3289, #7721, #7815, #10413, #16092, #14796, #3384, #9025, #7626, #14702, #697, #11986, #10599, #783, #6430, #16551, #16737, #2367, #9573, #12350, #13936, #6878, #971, #15337, #3921, #12259, #875, #18137, #1244, #13750, #5494, #18225, #9658, #11140, #12169, #1060, #2274, #2548, #7903, #4014, #12536, #6520, #13651, #2458, #5314, #8088, #6790, #16830, #4101, #13558, #17860, #6695, #18041, #2636, #8277, #10966, #1149, #14977, #15252, #16648, #8179, #13839, #12445, #7997, #5124, #5405, #11056, #10781, #16454, #3735, #9386, #15063, #3827, #6616, #17946, #5218, #10871, #9478, #15153, #12892, #10101, #112, #8363, #14023, #5585, #4283, #11231, #15433, #17012, #8443, #2815, #12718, #15784, #22, #14387, #12986, #300, #18314, #5673, #8714, #15691, #16919, #2989, #15598, #11496, #9926, #4195, #9752, #2900, #1691, #4464, #7325, #12806, #5942, #11591, #14113, #7234, #1426, #17287, #8534, #199, #14205, #5765, #1334, #2730, #1510, #9842, #7053, #17191, #6966, #15518, #12624, #11318, #7144, #11402, #17094, #4366, #10016, #8621, #14298, #1599, #5850, #3081, #6127, #16160, #17377, #3269, #11970, #11779, #6321, #10295, #17566, #1979, #3544, #14870, #8906, #4924, #11874, #1888, #8811, #7701, #9188, #3363, #13453, #7796, #17662, #765, #1790, #9008, #10197, #10486, #15876, #10575, #2164, #14491, #14583, #10390, #13267, #16068, #14775, #6410, #12055, #3173, #7422, #14683, #7606, #16251, #4557, #584, #9093, #13079, #4838, #6225, #3452, #2072, #13362, #15975, #397, #674, #6033, #11685, #4642, #7519, #13171, #485, #17473, #4742, #2255, #16339, #7880, #6676, #9547, #2525, #18112, #8061, #3631, #9280, #13537, #12237, #854, #5013, #6587, #16437, #10762, #2347, #5382, #7978, #3987, #2614, #8254, #6500, #13631, #16714, #5289, #12144, #10942, #5197, #1128, #17925, #17837, #17752, #10848, #9636, #12421, #15314, #2435, #13912, #1220, #3715, #15225, #9365, #6857, #16524, #8155, #3803, #13724, #14960, #10669, #9458, #5101, #15041, #6764 ),
 ( #13818, #15131, #943, #11031, #1035, #12329, #18015, #16625, #3900, #12691, #15496, #13997, #14535, #3220, #6944, #1934, #1486, #7120, #2793, #8424, #5742, #14086, #18206, #1398, #6074, #1312, #13126, #11292, #7026, #14631, #68, #12511, #5650, #15575, #5558, #8952, #16984, #5470, #1831, #11207, #12597, #3310, #11115, #8854, #4261, #15921, #9904, #2876, #8506, #16018, #7467, #2706, #4689, #14179, #16804, #12781, #17069, #10338, #18285, #89, #16896, #11382, #10243, #4172, #435, #4593, #4074, #11727, #9815, #17422, #9728, #15411, #8338, #7557, #529, #14723, #13213, #6176, #10436, #11824, #17521, #4783, #16113, #3405, #9047, #12592, #14078, #12414, #8501, #4067, #2519, #14173, #12504, #11024, #16798, #9717, #15404, #8418, #18197, #6937, #15307, #2700, #8331, #5552, #8147, #5463, #4254, #7782, #12321, #13992, #1305, #18279, #11200, #16889, #9541, #4166, #3892, #9630, #6669, #2606, #8245, #13811, #15569, #9810, #18010, #15491, #2788, #1392, #7018, #12685, #15218, #5644, #1121, #13906, #5280, #1214, #6850, #6756, #2869, #11286, #16979, #11108, #9898, #16618, #10936, #18106, #5375, #16706, #3980, #12207, #7763, #12024, #5072, #9335, #11940, #13599, #17893, #5165, #17538, #4893, #7943, #14933, #16133, #2225, #14836, #10728, #3512, #4805, #8975, #16217, #913, #3689, #6557, #17717, #10819, #16494, #7665, #6466, #645, #14649, #13423, #12115, #737, #4984, #13232, #1950, #9158, #10455, #13332, #16404, #7576, #14741, #549, #2040, #6193, #3423, #9064, #17633, #10638, #10542, #7852, #6286, #2133, #15012, #6380, #2309, #16311, #3597, #9248, #11842, #13506, #821, #17810, #11087, #1095, #8035, #6914, #8394, #2583, #12659, #6997, #16864, #18350, #1008, #8215, #9424, #9692, #15100, #11173, #14055, #13693, #2496, #9611, #12474, #15283, #13966, #5621, #1366, #2402, #6647, #13880, #6826, #4140, #9787, #1190, #8310, #11265, #16772, #18171, #5440, #4041, #15376, #1281, #3772, #10913, #2675, #16588, #12570, #18258, #3867, #15469, #5528, #12296, #2764, #8126, #9514, #15194, #17986, #13784, #5256, #6734, #12391, #18079, #5349, #11002, #16680, #3958, #14336, #4233, #5887, #57, #4501, #5978, #4314, #430, #1634, #12755, #6068, #4408, #2935, #8658, #7271, #12927, #339, #10049, #17227, #7183, #240, #11535, #15823, #5714, #15726, #14528, #10237, #9875, #10142, #3119, #8753, #14427, #1730, #1460, #7365, #14147, #1546, #16954, #12842, #146, #11354, #7461, #13025, #11630, #17130, #3025, #8476, #17324, #4588, #1824, #15914, #9961, #5796, #3212, #17043, #8848, #13121, #11439, #15635, #15550, #2846, #8570, #7090, #14242, #710, #2015, #14717, #4959, #7642, #17416, #621, #5049 ) ),
 .UNSPECIFIED., .F., .F., .F. ) 
 B_SPLINE_SURFACE_WITH_KNOTS ( ( 2, 2 ),
 ( 3, 2, 2, 2, 2, 2, 2, 2, 2, 2, 2, 2, 2, 2, 2, 2, 2, 2, 2, 2, 2, 2, 2, 2, 2, 2, 2, 2, 2, 2, 2, 2, 2, 2, 2, 2, 2, 2, 2, 2, 2, 2, 2, 2, 2, 2, 2, 2, 2, 2, 2, 2, 2, 2, 2, 2, 2, 2, 2, 2, 2, 2, 2, 2, 2, 2, 2, 2, 2, 2, 2, 2, 2, 2, 2, 2, 2, 2, 2, 2, 2, 2, 2, 2, 2, 2, 2, 2, 2, 2, 2, 2, 2, 2, 2, 2, 2, 2, 2, 2, 2, 2, 2, 2, 2, 2, 2, 2, 2, 2, 2, 2, 2, 2, 2, 2, 2, 2, 2, 2, 2, 2, 2, 2, 2, 2, 2, 2, 2, 2, 2, 2, 2, 2, 2, 2, 2, 2, 2, 2, 2, 2, 2, 2, 2, 2, 2, 2, 2, 2, 2, 2, 2, 2, 2, 2, 2, 2, 2, 2, 2, 2, 2, 2, 2, 2, 2, 2, 2, 2, 2, 2, 2, 2, 3 ),
 ( 0.000000000000000000, 1.000000000000000000 ),
 ( 0.000000000000000000, 0.005747126436781609116, 0.01149425287356321823, 0.01724137931034482735, 0.02298850574712643646, 0.02873563218390804558, 0.03448275862068965469, 0.04022988505747126381, 0.04597701149425287293, 0.05172413793103448204, 0.05747126436781609116, 0.06321839080459770721, 0.06896551724137930939, 0.07471264367816092544, 0.08045977011494252762, 0.08620689655172414367, 0.09195402298850574585, 0.09770114942528736190, 0.1034482758620689641, 0.1091954022988505801, 0.1149425287356321823, 0.1206896551724137984, 0.1264367816091954144, 0.1321839080459770166, 0.1379310344827586188, 0.1436781609195402210, 0.1494252873563218509, 0.1551724137931034531, 0.1609195402298850552, 0.1666666666666666574, 0.1724137931034482873, 0.1781609195402298895, 0.1839080459770114917, 0.1896551724137930939, 0.1954022988505747238, 0.2011494252873563260, 0.2068965517241379282, 0.2126436781609195303, 0.2183908045977011603, 0.2241379310344827624, 0.2298850574712643646, 0.2356321839080459668, 0.2413793103448275967, 0.2471264367816091989, 0.2528735632183908288, 0.2586206896551724310, 0.2643678160919540332, 0.2701149425287356354, 0.2758620689655172376, 0.2816091954022988397, 0.2873563218390804419, 0.2931034482758620441, 0.2988505747126437018, 0.3045977011494253039, 0.3103448275862069061, 0.3160919540229885083, 0.3218390804597701105, 0.3275862068965517127, 0.3333333333333333148, 0.3390804597701149170, 0.3448275862068965747, 0.3505747126436781769, 0.3563218390804597790, 0.3620689655172413812, 0.3678160919540229834, 0.3735632183908045856, 0.3793103448275861878, 0.3850574712643677899, 0.3908045977011494476, 0.3965517241379310498, 0.4022988505747126520, 0.4080459770114942541, 0.4137931034482758563, 0.4195402298850574585, 0.4252873563218390607, 0.4310344827586206629, 0.4367816091954023205, 0.4425287356321839227, 0.4482758620689655249, 0.4540229885057471271, 0.4597701149425287293, 0.4655172413793103314, 0.4712643678160919336, 0.4770114942528735358, 0.4827586206896551935, 0.4885057471264367956, 0.4942528735632183978, 0.5000000000000000000, 0.5057471264367816577, 0.5114942528735632044, 0.5172413793103448620, 0.5229885057471264087, 0.5287356321839080664, 0.5344827586206896131, 0.5402298850574712707, 0.5459770114942529284, 0.5517241379310344751, 0.5574712643678161328, 0.5632183908045976795, 0.5689655172413793371, 0.5747126436781608838, 0.5804597701149425415, 0.5862068965517240882, 0.5919540229885057459, 0.5977011494252874035, 0.6034482758620689502, 0.6091954022988506079, 0.6149425287356321546, 0.6206896551724138122, 0.6264367816091953589, 0.6321839080459770166, 0.6379310344827586743, 0.6436781609195402210, 0.6494252873563218786, 0.6551724137931034253, 0.6609195402298850830, 0.6666666666666666297, 0.6724137931034482873, 0.6781609195402298340, 0.6839080459770114917, 0.6896551724137931494, 0.6954022988505746961, 0.7011494252873563537, 0.7068965517241379004, 0.7126436781609195581, 0.7183908045977011048, 0.7241379310344827624, 0.7298850574712644201, 0.7356321839080459668, 0.7413793103448276245, 0.7471264367816091712, 0.7528735632183908288, 0.7586206896551723755, 0.7643678160919540332, 0.7701149425287355799, 0.7758620689655172376, 0.7816091954022988952, 0.7873563218390804419, 0.7931034482758620996, 0.7988505747126436463, 0.8045977011494253039, 0.8103448275862068506, 0.8160919540229885083, 0.8218390804597701660, 0.8275862068965517127, 0.8333333333333333703, 0.8390804597701149170, 0.8448275862068965747, 0.8505747126436781214, 0.8563218390804597790, 0.8620689655172413257, 0.8678160919540229834, 0.8735632183908046411, 0.8793103448275861878, 0.8850574712643678454, 0.8908045977011493921, 0.8965517241379310498, 0.9022988505747125965, 0.9080459770114942541, 0.9137931034482759118, 0.9195402298850574585, 0.9252873563218391162, 0.9310344827586206629, 0.9367816091954023205, 0.9425287356321838672, 0.9482758620689655249, 0.9540229885057470716, 0.9597701149425287293, 0.9655172413793103869, 0.9712643678160919336, 0.9770114942528735913, 0.9827586206896551380, 0.9885057471264367956, 0.9942528735632183423, 0.9961881922148684287 ),
 .UNSPECIFIED. ) 
 GEOMETRIC_REPRESENTATION_ITEM ( )  RATIONAL_B_SPLINE_SURFACE ( (
 ( 1.000000000000000000, 0.8660254037844387076, 1.000000000000000000, 0.8660254037844387076, 1.000000000000000000, 0.8660254037844387076, 1.000000000000000000, 0.8660254037844387076, 1.000000000000000000, 0.8660254037844387076, 1.000000000000000000, 0.8660254037844387076, 1.000000000000000000, 0.8660254037844387076, 1.000000000000000000, 0.8660254037844387076, 1.000000000000000000, 0.8660254037844387076, 1.000000000000000000, 0.8660254037844387076, 1.000000000000000000, 0.8660254037844387076, 1.000000000000000000, 0.8660254037844387076, 1.000000000000000000, 0.8660254037844387076, 1.000000000000000000, 0.8660254037844387076, 1.000000000000000000, 0.8660254037844387076, 1.000000000000000000, 0.8660254037844387076, 1.000000000000000000, 0.8660254037844387076, 1.000000000000000000, 0.8660254037844387076, 1.000000000000000000, 0.8660254037844387076, 1.000000000000000000, 0.8660254037844387076, 1.000000000000000000, 0.8660254037844387076, 1.000000000000000000, 0.8660254037844387076, 1.000000000000000000, 0.8660254037844387076, 1.000000000000000000, 0.8660254037844387076, 1.000000000000000000, 0.8660254037844387076, 1.000000000000000000, 0.8660254037844387076, 1.000000000000000000, 0.8660254037844387076, 1.000000000000000000, 0.8660254037844387076, 1.000000000000000000, 0.8660254037844387076, 1.000000000000000000, 0.8660254037844387076, 1.000000000000000000, 0.8660254037844387076, 1.000000000000000000, 0.8660254037844387076, 1.000000000000000000, 0.8660254037844387076, 1.000000000000000000, 0.8660254037844387076, 1.000000000000000000, 0.8660254037844387076, 1.000000000000000000, 0.8660254037844387076, 1.000000000000000000, 0.8660254037844387076, 1.000000000000000000, 0.8660254037844387076, 1.000000000000000000, 0.8660254037844387076, 1.000000000000000000, 0.8660254037844387076, 1.000000000000000000, 0.8660254037844387076, 1.000000000000000000, 0.8660254037844387076, 1.000000000000000000, 0.8660254037844387076, 1.000000000000000000, 0.8660254037844387076, 1.000000000000000000, 0.8660254037844387076, 1.000000000000000000, 0.8660254037844387076, 1.000000000000000000, 0.8660254037844387076, 1.000000000000000000, 0.8660254037844387076, 1.000000000000000000, 0.8660254037844387076, 1.000000000000000000, 0.8660254037844387076, 1.000000000000000000, 0.8660254037844387076, 1.000000000000000000, 0.8660254037844387076, 1.000000000000000000, 0.8660254037844387076, 1.000000000000000000, 0.8660254037844387076, 1.000000000000000000, 0.8660254037844387076, 1.000000000000000000, 0.8660254037844387076, 1.000000000000000000, 0.8660254037844387076, 1.000000000000000000, 0.8660254037844387076, 1.000000000000000000, 0.8660254037844387076, 1.000000000000000000, 0.8660254037844387076, 1.000000000000000000, 0.8660254037844387076, 1.000000000000000000, 0.8660254037844387076, 1.000000000000000000, 0.8660254037844387076, 1.000000000000000000, 0.8660254037844387076, 1.000000000000000000, 0.8660254037844387076, 1.000000000000000000, 0.8660254037844387076, 1.000000000000000000, 0.8660254037844387076, 1.000000000000000000, 0.8660254037844387076, 1.000000000000000000, 0.8660254037844387076, 1.000000000000000000, 0.8660254037844387076, 1.000000000000000000, 0.8660254037844387076, 1.000000000000000000, 0.8660254037844387076, 1.000000000000000000, 0.8660254037844387076, 1.000000000000000000, 0.8660254037844387076, 1.000000000000000000, 0.8660254037844387076, 1.000000000000000000, 0.8660254037844387076, 1.000000000000000000, 0.8660254037844387076, 1.000000000000000000, 0.8660254037844387076, 1.000000000000000000, 0.8660254037844387076, 1.000000000000000000, 0.8660254037844387076, 1.000000000000000000, 0.8660254037844387076, 1.000000000000000000, 0.8660254037844387076, 1.000000000000000000, 0.8660254037844387076, 1.000000000000000000, 0.8660254037844387076, 1.000000000000000000, 0.8660254037844387076, 1.000000000000000000, 0.8660254037844387076, 1.000000000000000000, 0.8660254037844387076, 1.000000000000000000, 0.8660254037844387076, 1.000000000000000000, 0.8660254037844387076, 1.000000000000000000, 0.8660254037844387076, 1.000000000000000000, 0.8660254037844387076, 1.000000000000000000, 0.8660254037844387076, 1.000000000000000000, 0.8660254037844387076, 1.000000000000000000, 0.8660254037844387076, 1.000000000000000000, 0.8660254037844387076, 1.000000000000000000, 0.8660254037844387076, 1.000000000000000000, 0.8660254037844387076, 1.000000000000000000, 0.8660254037844387076, 1.000000000000000000, 0.8660254037844387076, 1.000000000000000000, 0.8660254037844387076, 1.000000000000000000, 0.8660254037844387076, 1.000000000000000000, 0.8660254037844387076, 1.000000000000000000, 0.8660254037844387076, 1.000000000000000000, 0.8660254037844387076, 1.000000000000000000, 0.8660254037844387076, 1.000000000000000000, 0.8660254037844387076, 1.000000000000000000, 0.8660254037844387076, 1.000000000000000000, 0.8660254037844387076, 1.000000000000000000, 0.8660254037844387076, 1.000000000000000000, 0.8660254037844387076, 1.000000000000000000, 0.8660254037844387076, 1.000000000000000000, 0.8660254037844387076, 1.000000000000000000, 0.8660254037844387076, 1.000000000000000000, 0.8660254037844387076, 1.000000000000000000, 0.8660254037844387076, 1.000000000000000000, 0.8660254037844387076, 1.000000000000000000, 0.8660254037844387076, 1.000000000000000000, 0.8660254037844387076, 1.000000000000000000, 0.8660254037844387076, 1.000000000000000000, 0.8660254037844387076, 1.000000000000000000, 0.8660254037844387076, 1.000000000000000000, 0.8660254037844387076, 1.000000000000000000, 0.8660254037844387076, 1.000000000000000000, 0.8660254037844387076, 1.000000000000000000, 0.8660254037844387076, 1.000000000000000000, 0.8660254037844387076, 1.000000000000000000, 0.8660254037844387076, 1.000000000000000000, 0.8660254037844387076, 1.000000000000000000, 0.8660254037844387076, 1.000000000000000000, 0.8660254037844387076, 1.000000000000000000, 0.8660254037844387076, 1.000000000000000000, 0.8660254037844387076, 1.000000000000000000, 0.8660254037844387076, 1.000000000000000000, 0.8660254037844387076, 1.000000000000000000, 0.8660254037844387076, 1.000000000000000000, 0.8660254037844387076, 1.000000000000000000, 0.8660254037844387076, 1.000000000000000000, 0.8660254037844387076, 1.000000000000000000, 0.8660254037844387076, 1.000000000000000000, 0.8660254037844387076, 1.000000000000000000, 0.8660254037844387076, 1.000000000000000000, 0.8660254037844387076, 1.000000000000000000, 0.8660254037844387076, 1.000000000000000000, 0.8660254037844387076, 1.000000000000000000, 0.8660254037844387076, 1.000000000000000000, 0.8660254037844387076, 1.000000000000000000, 0.8660254037844387076, 1.000000000000000000, 0.8660254037844387076, 1.000000000000000000, 0.8660254037844387076, 1.000000000000000000, 0.8660254037844387076, 1.000000000000000000, 0.8660254037844387076, 1.000000000000000000, 0.8660254037844387076, 1.000000000000000000, 0.8660254037844387076, 1.000000000000000000, 0.8660254037844387076, 1.000000000000000000, 0.8660254037844387076, 1.000000000000000000, 0.8660254037844387076, 1.000000000000000000, 0.8660254037844387076, 1.000000000000000000, 0.8660254037844387076, 1.000000000000000000, 0.8660254037844387076, 1.000000000000000000, 0.8660254037844387076, 1.000000000000000000, 0.8660254037844387076, 1.000000000000000000, 0.8660254037844387076, 1.000000000000000000, 0.8660254037844387076, 1.000000000000000000, 0.8660254037844387076, 1.000000000000000000, 0.8660254037844387076, 1.000000000000000000, 0.8660254037844387076, 1.000000000000000000, 0.8660254037844387076, 1.000000000000000000, 0.8660254037844387076, 1.000000000000000000, 0.8660254037844387076, 1.000000000000000000, 0.8660254037844387076, 1.000000000000000000, 0.8660254037844387076, 1.000000000000000000, 0.8660254037844387076, 1.000000000000000000, 0.8660254037844387076, 1.000000000000000000, 0.9548846649268323272, 0.9401540970596700131),
 ( 1.000000000000000000, 0.8660254037844387076, 1.000000000000000000, 0.8660254037844387076, 1.000000000000000000, 0.8660254037844387076, 1.000000000000000000, 0.8660254037844387076, 1.000000000000000000, 0.8660254037844387076, 1.000000000000000000, 0.8660254037844387076, 1.000000000000000000, 0.8660254037844387076, 1.000000000000000000, 0.8660254037844387076, 1.000000000000000000, 0.8660254037844387076, 1.000000000000000000, 0.8660254037844387076, 1.000000000000000000, 0.8660254037844387076, 1.000000000000000000, 0.8660254037844387076, 1.000000000000000000, 0.8660254037844387076, 1.000000000000000000, 0.8660254037844387076, 1.000000000000000000, 0.8660254037844387076, 1.000000000000000000, 0.8660254037844387076, 1.000000000000000000, 0.8660254037844387076, 1.000000000000000000, 0.8660254037844387076, 1.000000000000000000, 0.8660254037844387076, 1.000000000000000000, 0.8660254037844387076, 1.000000000000000000, 0.8660254037844387076, 1.000000000000000000, 0.8660254037844387076, 1.000000000000000000, 0.8660254037844387076, 1.000000000000000000, 0.8660254037844387076, 1.000000000000000000, 0.8660254037844387076, 1.000000000000000000, 0.8660254037844387076, 1.000000000000000000, 0.8660254037844387076, 1.000000000000000000, 0.8660254037844387076, 1.000000000000000000, 0.8660254037844387076, 1.000000000000000000, 0.8660254037844387076, 1.000000000000000000, 0.8660254037844387076, 1.000000000000000000, 0.8660254037844387076, 1.000000000000000000, 0.8660254037844387076, 1.000000000000000000, 0.8660254037844387076, 1.000000000000000000, 0.8660254037844387076, 1.000000000000000000, 0.8660254037844387076, 1.000000000000000000, 0.8660254037844387076, 1.000000000000000000, 0.8660254037844387076, 1.000000000000000000, 0.8660254037844387076, 1.000000000000000000, 0.8660254037844387076, 1.000000000000000000, 0.8660254037844387076, 1.000000000000000000, 0.8660254037844387076, 1.000000000000000000, 0.8660254037844387076, 1.000000000000000000, 0.8660254037844387076, 1.000000000000000000, 0.8660254037844387076, 1.000000000000000000, 0.8660254037844387076, 1.000000000000000000, 0.8660254037844387076, 1.000000000000000000, 0.8660254037844387076, 1.000000000000000000, 0.8660254037844387076, 1.000000000000000000, 0.8660254037844387076, 1.000000000000000000, 0.8660254037844387076, 1.000000000000000000, 0.8660254037844387076, 1.000000000000000000, 0.8660254037844387076, 1.000000000000000000, 0.8660254037844387076, 1.000000000000000000, 0.8660254037844387076, 1.000000000000000000, 0.8660254037844387076, 1.000000000000000000, 0.8660254037844387076, 1.000000000000000000, 0.8660254037844387076, 1.000000000000000000, 0.8660254037844387076, 1.000000000000000000, 0.8660254037844387076, 1.000000000000000000, 0.8660254037844387076, 1.000000000000000000, 0.8660254037844387076, 1.000000000000000000, 0.8660254037844387076, 1.000000000000000000, 0.8660254037844387076, 1.000000000000000000, 0.8660254037844387076, 1.000000000000000000, 0.8660254037844387076, 1.000000000000000000, 0.8660254037844387076, 1.000000000000000000, 0.8660254037844387076, 1.000000000000000000, 0.8660254037844387076, 1.000000000000000000, 0.8660254037844387076, 1.000000000000000000, 0.8660254037844387076, 1.000000000000000000, 0.8660254037844387076, 1.000000000000000000, 0.8660254037844387076, 1.000000000000000000, 0.8660254037844387076, 1.000000000000000000, 0.8660254037844387076, 1.000000000000000000, 0.8660254037844387076, 1.000000000000000000, 0.8660254037844387076, 1.000000000000000000, 0.8660254037844387076, 1.000000000000000000, 0.8660254037844387076, 1.000000000000000000, 0.8660254037844387076, 1.000000000000000000, 0.8660254037844387076, 1.000000000000000000, 0.8660254037844387076, 1.000000000000000000, 0.8660254037844387076, 1.000000000000000000, 0.8660254037844387076, 1.000000000000000000, 0.8660254037844387076, 1.000000000000000000, 0.8660254037844387076, 1.000000000000000000, 0.8660254037844387076, 1.000000000000000000, 0.8660254037844387076, 1.000000000000000000, 0.8660254037844387076, 1.000000000000000000, 0.8660254037844387076, 1.000000000000000000, 0.8660254037844387076, 1.000000000000000000, 0.8660254037844387076, 1.000000000000000000, 0.8660254037844387076, 1.000000000000000000, 0.8660254037844387076, 1.000000000000000000, 0.8660254037844387076, 1.000000000000000000, 0.8660254037844387076, 1.000000000000000000, 0.8660254037844387076, 1.000000000000000000, 0.8660254037844387076, 1.000000000000000000, 0.8660254037844387076, 1.000000000000000000, 0.8660254037844387076, 1.000000000000000000, 0.8660254037844387076, 1.000000000000000000, 0.8660254037844387076, 1.000000000000000000, 0.8660254037844387076, 1.000000000000000000, 0.8660254037844387076, 1.000000000000000000, 0.8660254037844387076, 1.000000000000000000, 0.8660254037844387076, 1.000000000000000000, 0.8660254037844387076, 1.000000000000000000, 0.8660254037844387076, 1.000000000000000000, 0.8660254037844387076, 1.000000000000000000, 0.8660254037844387076, 1.000000000000000000, 0.8660254037844387076, 1.000000000000000000, 0.8660254037844387076, 1.000000000000000000, 0.8660254037844387076, 1.000000000000000000, 0.8660254037844387076, 1.000000000000000000, 0.8660254037844387076, 1.000000000000000000, 0.8660254037844387076, 1.000000000000000000, 0.8660254037844387076, 1.000000000000000000, 0.8660254037844387076, 1.000000000000000000, 0.8660254037844387076, 1.000000000000000000, 0.8660254037844387076, 1.000000000000000000, 0.8660254037844387076, 1.000000000000000000, 0.8660254037844387076, 1.000000000000000000, 0.8660254037844387076, 1.000000000000000000, 0.8660254037844387076, 1.000000000000000000, 0.8660254037844387076, 1.000000000000000000, 0.8660254037844387076, 1.000000000000000000, 0.8660254037844387076, 1.000000000000000000, 0.8660254037844387076, 1.000000000000000000, 0.8660254037844387076, 1.000000000000000000, 0.8660254037844387076, 1.000000000000000000, 0.8660254037844387076, 1.000000000000000000, 0.8660254037844387076, 1.000000000000000000, 0.8660254037844387076, 1.000000000000000000, 0.8660254037844387076, 1.000000000000000000, 0.8660254037844387076, 1.000000000000000000, 0.8660254037844387076, 1.000000000000000000, 0.8660254037844387076, 1.000000000000000000, 0.8660254037844387076, 1.000000000000000000, 0.8660254037844387076, 1.000000000000000000, 0.8660254037844387076, 1.000000000000000000, 0.8660254037844387076, 1.000000000000000000, 0.8660254037844387076, 1.000000000000000000, 0.8660254037844387076, 1.000000000000000000, 0.8660254037844387076, 1.000000000000000000, 0.8660254037844387076, 1.000000000000000000, 0.8660254037844387076, 1.000000000000000000, 0.8660254037844387076, 1.000000000000000000, 0.8660254037844387076, 1.000000000000000000, 0.8660254037844387076, 1.000000000000000000, 0.8660254037844387076, 1.000000000000000000, 0.8660254037844387076, 1.000000000000000000, 0.8660254037844387076, 1.000000000000000000, 0.8660254037844387076, 1.000000000000000000, 0.8660254037844387076, 1.000000000000000000, 0.8660254037844387076, 1.000000000000000000, 0.8660254037844387076, 1.000000000000000000, 0.8660254037844387076, 1.000000000000000000, 0.8660254037844387076, 1.000000000000000000, 0.8660254037844387076, 1.000000000000000000, 0.8660254037844387076, 1.000000000000000000, 0.8660254037844387076, 1.000000000000000000, 0.8660254037844387076, 1.000000000000000000, 0.8660254037844387076, 1.000000000000000000, 0.8660254037844387076, 1.000000000000000000, 0.8660254037844387076, 1.000000000000000000, 0.8660254037844387076, 1.000000000000000000, 0.8660254037844387076, 1.000000000000000000, 0.8660254037844387076, 1.000000000000000000, 0.8660254037844387076, 1.000000000000000000, 0.8660254037844387076, 1.000000000000000000, 0.8660254037844387076, 1.000000000000000000, 0.8660254037844387076, 1.000000000000000000, 0.8660254037844387076, 1.000000000000000000, 0.9548846649268323272, 0.9401540970596700131) ) ) 
 REPRESENTATION_ITEM ( '' )  SURFACE ( )  );
#11829 = VERTEX_POINT ( 'NONE', #18054 ) ;
#11830 = CARTESIAN_POINT ( 'NONE',  ( -5.330712181944246111E-15, -27.33340804591119522, -6.211691927533303570 ) ) ;
#11831 = CARTESIAN_POINT ( 'NONE',  ( 4.518350579753633411, 39.37180007765647360, 1.405661355842698468 ) ) ;
#11832 = ORIENTED_EDGE ( 'NONE', *, *, #10205, .F. ) ;
#11833 = DIRECTION ( 'NONE',  ( 0.000000000000000000, 1.000000000000000000, 0.000000000000000000 ) ) ;
#11834 = DIRECTION ( 'NONE',  ( -0.000000000000000000, 1.000000000000000000, -0.000000000000000000 ) ) ;
#11835 = CARTESIAN_POINT ( 'NONE',  ( 2.121784821875004390, -22.78265288675364175, -14.66275540855586890 ) ) ;
#11836 = CARTESIAN_POINT ( 'NONE',  ( -8.000000000000001776, 27.59999999999999432, 2.499999999999998224 ) ) ;
#11837 = CARTESIAN_POINT ( 'NONE',  ( -4.000000000000004441, -27.72246025710361295, -11.28397838367063244 ) ) ;
#11838 = CARTESIAN_POINT ( 'NONE',  ( 4.730628863548789710E-15, -16.33737451245578498, -7.593689001224928958 ) ) ;
#11839 = ORIENTED_EDGE ( 'NONE', *, *, #3378, .F. ) ;
#11840 = CARTESIAN_POINT ( 'NONE',  ( -4.000000000000004441, -25.39947568988189985, -7.966412604300202815 ) ) ;
#11841 = EDGE_CURVE ( 'NONE', #14660, #12399, #2197, .T. ) ;
#11842 = CARTESIAN_POINT ( 'NONE',  ( -3.999999999999997335, -20.62655511095648109, -9.202611407326488191 ) ) ;
#11843 = AXIS2_PLACEMENT_3D ( 'NONE', #616, #2196, #11994 ) ;
#11844 = DIRECTION ( 'NONE',  ( 0.000000000000000000, 0.000000000000000000, -1.000000000000000000 ) ) ;
#11845 = EDGE_LOOP ( 'NONE', ( #14021, #15516 ) ) ;
#11846 = EDGE_LOOP ( 'NONE', ( #14053, #14755 ) ) ;
#11847 = CARTESIAN_POINT ( 'NONE',  ( 3.579096709490575479E-14, -24.61191250054342916, -3.894186529857098567 ) ) ;
#11848 = DIRECTION ( 'NONE',  ( -0.000000000000000000, 1.000000000000000000, 0.000000000000000000 ) ) ;
#11849 = CARTESIAN_POINT ( 'NONE',  ( -4.499999999999999112, 24.50319992234354771, -0.05647727720528529505 ) ) ;
#11850 = CARTESIAN_POINT ( 'NONE',  ( 0.05938372350920110426, 32.62819992234354771, -3.680117784833935701 ) ) ;
#11851 = CARTESIAN_POINT ( 'NONE',  ( -0.7188294034286550893, 17.50319992234354771, -2.395093729190349130 ) ) ;
#11852 = EDGE_LOOP ( 'NONE', ( #1192, #2360, #10963, #2890 ) ) ;
#11853 = CARTESIAN_POINT ( 'NONE',  ( 0.05938372350929014415, 19.87180007765647716, 4.731580009072201776 ) ) ;
#11854 = CARTESIAN_POINT ( 'NONE',  ( -3.999999999999997335, -20.82013715752001559, -9.479075221267256879 ) ) ;
#11855 = ORIENTED_EDGE ( 'NONE', *, *, #10050, .F. ) ;
#11856 = AXIS2_PLACEMENT_3D ( 'NONE', #18215, #15421, #15142 ) ;
#11857 = DIRECTION ( 'NONE',  ( 0.000000000000000000, -0.5735764363510547081, -0.8191520442889856923 ) ) ;
#11858 = CARTESIAN_POINT ( 'NONE',  ( 3.518350579753631191, 26.87180007765647360, 1.080741659609802285 ) ) ;
#11859 = ADVANCED_FACE ( 'NONE', ( #5328 ), #2470, .T. ) ;
#11860 = LINE ( 'NONE', #17458, #2235 ) ;
#11861 = CARTESIAN_POINT ( 'NONE',  ( 4.243569643750000786, -20.89974471738585748, -5.566448692132691001 ) ) ;
#11862 = CARTESIAN_POINT ( 'NONE',  ( 4.243569643750000786, -24.54553994094216307, -10.77318387364461572 ) ) ;
#11863 = EDGE_CURVE ( 'NONE', #9924, #16667, #11995, .T. ) ;
#11864 = CARTESIAN_POINT ( 'NONE',  ( 1.999999999999994449, -29.37813640364300127, -11.63537001862205855 ) ) ;
#11865 = ORIENTED_EDGE ( 'NONE', *, *, #2210, .F. ) ;
#11866 = CARTESIAN_POINT ( 'NONE',  ( 3.678256433395794112, -9.999999999998108180, 21.51556408013178157 ) ) ;
#11867 = DIRECTION ( 'NONE',  ( 0.000000000000000000, -1.000000000000000000, 0.000000000000000000 ) ) ;
#11868 = CARTESIAN_POINT ( 'NONE',  ( -5.577813053751546416E-15, -25.45076803941176991, -5.092196395636519490 ) ) ;
#11869 = SURFACE_STYLE_USAGE ( .BOTH. , #7417 ) ;
#11870 = ORIENTED_EDGE ( 'NONE', *, *, #3497, .F. ) ;
#11871 = VECTOR ( 'NONE', #13307, 1000.000000000000000 ) ;
#11872 = CARTESIAN_POINT ( 'NONE',  ( -3.500000000000000444, 27.00319992234354771, -0.05647727720529563400 ) ) ;
#11873 = CARTESIAN_POINT ( 'NONE',  ( 4.005420803925811235, -27.01550616763517709, -14.30066121701663029 ) ) ;
#11874 = CARTESIAN_POINT ( 'NONE',  ( -2.121784821874996396, -18.83573003411303048, -9.025965403792225672 ) ) ;
#11875 = CARTESIAN_POINT ( 'NONE',  ( 2.500000000000001332, 19.24680007765648071, -0.05647727720535888202 ) ) ;
#11876 = AXIS2_PLACEMENT_3D ( 'NONE', #15627, #4400, #8384 ) ;
#11877 = CARTESIAN_POINT ( 'NONE',  ( 2.829195390882724759, 17.87819992234354416, -3.793023760679264278 ) ) ;
#11878 = CARTESIAN_POINT ( 'NONE',  ( -1.999999999999996225, -23.25119311998180649, -14.96414190187491400 ) ) ;
#11879 = CARTESIAN_POINT ( 'NONE',  ( 4.243569643749996345, -22.96046137712846047, -4.237966970562988323 ) ) ;
#11880 = CARTESIAN_POINT ( 'NONE',  ( -7.082115535667631079, -12.11711825479596172, 11.44395564418984002 ) ) ;
#11881 = VECTOR ( 'NONE', #14690, 1000.000000000000000 ) ;
#11882 = EDGE_CURVE ( 'NONE', #10922, #5047, #9310, .T. ) ;
#11883 = CARTESIAN_POINT ( 'NONE',  ( 13.80999999999999872, 0.000000000000000000, 2.000000000000000444 ) ) ;
#11884 = LINE ( 'NONE', #12158, #2971 ) ;
#11885 = CARTESIAN_POINT ( 'NONE',  ( -1.071796769724486564, -27.97886135391585682, -8.702687823603630690 ) ) ;
#11886 = ORIENTED_EDGE ( 'NONE', *, *, #2441, .T. ) ;
#11887 = ORIENTED_EDGE ( 'NONE', *, *, #4909, .F. ) ;
#11888 = DIRECTION ( 'NONE',  ( 0.000000000000000000, 0.000000000000000000, 1.000000000000000000 ) ) ;
#11889 = FACE_OUTER_BOUND ( 'NONE', #8766, .T. ) ;
#11890 = FACE_BOUND ( 'NONE', #8128, .T. ) ;
#11891 = EDGE_LOOP ( 'NONE', ( #14598, #15319, #8296, #16978 ) ) ;
#11892 = CARTESIAN_POINT ( 'NONE',  ( -0.05938372350921170689, 31.37819992234354061, 2.628655560595669183 ) ) ;
#11893 = FILL_AREA_STYLE ('',( #1998 ) ) ;
#11894 = CARTESIAN_POINT ( 'NONE',  ( 4.243569643750003451, -24.03347965934736763, -14.31337611479460037 ) ) ;
#11895 = CARTESIAN_POINT ( 'NONE',  ( -1.027846397803541700, 24.99680007765647716, 3.346150245485522312 ) ) ;
#11896 = STYLED_ITEM ( 'NONE', ( #12029 ), #3417 ) ;
#11897 = PLANE ( 'NONE',  #9287 ) ;
#11898 = CARTESIAN_POINT ( 'NONE',  ( 2.237551826325104631, -10.00000000000000178, -12.18738508574795176 ) ) ;
#11899 = AXIS2_PLACEMENT_3D ( 'NONE', #1044, #18024, #3907 ) ;
#11900 = CARTESIAN_POINT ( 'NONE',  ( -2.121784821875005722, -28.15821100236278696, -9.525377681565375454 ) ) ;
#11901 = AXIS2_PLACEMENT_3D ( 'NONE', #9986, #15848, #7297 ) ;
#11902 = CARTESIAN_POINT ( 'NONE',  ( -2.000000000000005773, -27.03364271935316765, -8.287086036584028648 ) ) ;
#11903 = CIRCLE ( 'NONE', #13083, 10.00000000000000000 ) ;
#11904 = CARTESIAN_POINT ( 'NONE',  ( 4.243569643750003451, -22.48482328119956009, -12.10166559521431573 ) ) ;
#11905 =( BOUNDED_CURVE ( )  B_SPLINE_CURVE ( 3, ( #3905, #8160, #12519, #8696 ),
 .UNSPECIFIED., .F., .F. ) 
 B_SPLINE_CURVE_WITH_KNOTS ( ( 4, 4 ),
 ( 8.673617379884036458E-16, 1.570796326794896558 ),
 .UNSPECIFIED. ) 
 CURVE ( )  GEOMETRIC_REPRESENTATION_ITEM ( )  RATIONAL_B_SPLINE_CURVE ( ( 1.000000000000000000, 0.8047378541243652705, 0.8047378541243652705, 1.000000000000000000 ) ) 
 REPRESENTATION_ITEM ( '' )  );
#11906 = CARTESIAN_POINT ( 'NONE',  ( -1.734723475976807094E-15, 25.39999999999999503, -12.50000000000000000 ) ) ;
#11907 =( GEOMETRIC_REPRESENTATION_CONTEXT ( 3 ) GLOBAL_UNCERTAINTY_ASSIGNED_CONTEXT ( ( #12376 ) ) GLOBAL_UNIT_ASSIGNED_CONTEXT ( ( #14154, #15381, #11005 ) ) REPRESENTATION_CONTEXT ( 'NONE', 'WORKASPACE' ) );
#11908 = CARTESIAN_POINT ( 'NONE',  ( 0.000000000000000000, 1.759474945355381514, -3.047500000000001652 ) ) ;
#11909 = DIRECTION ( 'NONE',  ( 0.000000000000000000, 0.000000000000000000, 1.000000000000000000 ) ) ;
#11910 = CARTESIAN_POINT ( 'NONE',  ( -2.121784821875005722, -26.06107215695429247, -6.530353019633736267 ) ) ;
#11911 = CARTESIAN_POINT ( 'NONE',  ( -6.158835246850665095E-15, -22.64013793229036509, -15.02577497543054186 ) ) ;
#11912 = CARTESIAN_POINT ( 'NONE',  ( 0.000000000000000000, 0.7216878364870329410, 1.249999999999999778 ) ) ;
#11913 = CARTESIAN_POINT ( 'NONE',  ( 2.518350579753628971, 31.87180007765648426, 0.7558219633769073242 ) ) ;
#11914 = EDGE_LOOP ( 'NONE', ( #17086, #11886, #6336, #227 ) ) ;
#11915 = CARTESIAN_POINT ( 'NONE',  ( -2.798362969681365886, 32.74680007765648071, 2.102939460078824929 ) ) ;
#11916 = DIRECTION ( 'NONE',  ( -0.000000000000000000, 1.000000000000000000, -0.000000000000000000 ) ) ;
#11917 = ADVANCED_FACE ( 'NONE', ( #9583 ), #793, .T. ) ;
#11918 = VECTOR ( 'NONE', #16316, 1000.000000000000000 ) ;
#11919 = CARTESIAN_POINT ( 'NONE',  ( 3.999999999999996447, -22.21612646813362346, -3.420118758496274225 ) ) ;
#11920 = EDGE_CURVE ( 'NONE', #18081, #17590, #10609, .T. ) ;
#11921 = CARTESIAN_POINT ( 'NONE',  ( -0.05938372350920063936, 18.87819992234354771, 3.680117784833935701 ) ) ;
#11922 = ORIENTED_EDGE ( 'NONE', *, *, #14431, .F. ) ;
#11923 = CARTESIAN_POINT ( 'NONE',  ( 4.243569643750003451, -20.45221178488055713, -9.198795538265191141 ) ) ;
#11924 = EDGE_CURVE ( 'NONE', #8582, #894, #16235, .T. ) ;
#11925 = CARTESIAN_POINT ( 'NONE',  ( -1.444289557196047014, 38.49680007765647360, -4.262301884875704161 ) ) ;
#11926 = VERTEX_POINT ( 'NONE', #15073 ) ;
#11927 = EDGE_CURVE ( 'NONE', #6687, #18210, #5228, .T. ) ;
#11928 = DIRECTION ( 'NONE',  ( 0.000000000000000000, 0.000000000000000000, -1.000000000000000000 ) ) ;
#11929 = CARTESIAN_POINT ( 'NONE',  ( -8.500000000000010658, 15.00000000000000178, 20.49999999999998934 ) ) ;
#11930 = CARTESIAN_POINT ( 'NONE',  ( -4.243569643750005227, -27.17624818430860856, -10.25873449608710608 ) ) ;
#11931 = CARTESIAN_POINT ( 'NONE',  ( -1.071796769724496334, -28.55960749642623142, -9.532079269453008763 ) ) ;
#11932 = AXIS2_PLACEMENT_3D ( 'NONE', #6897, #7233, #484 ) ;
#11933 = DIRECTION ( 'NONE',  ( -1.000000000000000000, 0.000000000000000000, -0.000000000000000000 ) ) ;
#11934 = AXIS2_PLACEMENT_3D ( 'NONE', #6852, #5282, #11110 ) ;
#11935 = CARTESIAN_POINT ( 'NONE',  ( 1.999999999999994449, -25.44196810847903478, -6.013939113682064352 ) ) ;
#11936 = CARTESIAN_POINT ( 'NONE',  ( 4.730628863548789710E-15, -16.07926511609781528, -7.225070581294880334 ) ) ;
#11937 = EDGE_CURVE ( 'NONE', #4967, #1717, #12950, .T. ) ;
#11938 = EDGE_LOOP ( 'NONE', ( #12714, #14127, #9109, #9641 ) ) ;
#11939 = CARTESIAN_POINT ( 'NONE',  ( 1.999999999999994449, -26.02271425098940938, -6.843330559531437984 ) ) ;
#11940 = CARTESIAN_POINT ( 'NONE',  ( 1.999999999999994449, -26.53893304370534523, -7.580567399391532568 ) ) ;
#11941 = ORIENTED_EDGE ( 'NONE', *, *, #9265, .F. ) ;
#11942 =( BOUNDED_CURVE ( )  B_SPLINE_CURVE ( 2, ( #12554, #18239, #5509, #10124, #7346, #15708, #5605, #11250, #127 ),
 .UNSPECIFIED., .F., .T. ) 
 B_SPLINE_CURVE_WITH_KNOTS ( ( 3, 2, 2, 2, 3 ),
 ( 0.6637931034482759118, 0.6666666666666666297, 0.6724137931034482873, 0.6781609195402298340, 0.6810344827586206629 ),
 .UNSPECIFIED. ) 
 CURVE ( )  GEOMETRIC_REPRESENTATION_ITEM ( )  RATIONAL_B_SPLINE_CURVE ( ( 0.9330127018922194093, 0.9330127018922206306, 1.000000000000000000, 0.8660254037844387076, 1.000000000000000000, 0.8660254037844387076, 1.000000000000000000, 0.9330127018922194093, 0.9330127018922194093 ) ) 
 REPRESENTATION_ITEM ( '' )  );
#11943 = ORIENTED_EDGE ( 'NONE', *, *, #85, .F. ) ;
#11944 = CARTESIAN_POINT ( 'NONE',  ( 8.399999999999998579, 0.000000000000000000, 0.000000000000000000 ) ) ;
#11945 = PRODUCT_DEFINITION ( 'UNKNOWN', '', #12792, #7970 ) ;
#11946 = FACE_OUTER_BOUND ( 'NONE', #11049, .T. ) ;
#11947 = CARTESIAN_POINT ( 'NONE',  ( 4.481649420246397675, 23.37819992234354416, 1.518615910253363177 ) ) ;
#11948 = CARTESIAN_POINT ( 'NONE',  ( 2.211161402132839182, 35.37819992234354061, -2.942372952327217739 ) ) ;
#11949 = CARTESIAN_POINT ( 'NONE',  ( -1.989345975306457071, 22.25319992234354771, -1.515154207786300944 ) ) ;
#11950 = VECTOR ( 'NONE', #11446, 1000.000000000000000 ) ;
#11951 = ORIENTED_EDGE ( 'NONE', *, *, #3061, .T. ) ;
#11952 = CARTESIAN_POINT ( 'NONE',  ( 1.444289557196047680, 19.74680007765647716, 4.262301884875704161 ) ) ;
#11953 = CARTESIAN_POINT ( 'NONE',  ( -5.279047395330986450E-15, -25.37691494596528941, -3.907874615766512960 ) ) ;
#11954 = ORIENTED_EDGE ( 'NONE', *, *, #4671, .T. ) ;
#11955 = DIRECTION ( 'NONE',  ( 0.000000000000000000, 0.000000000000000000, -1.000000000000000000 ) ) ;
#11956 = CARTESIAN_POINT ( 'NONE',  ( 0.05938372350927906274, 39.87180007765648071, 3.680117784833935701 ) ) ;
#11957 = DIRECTION ( 'NONE',  ( 3.469446951953612217E-16, -0.000000000000000000, 1.000000000000000000 ) ) ;
#11958 = CARTESIAN_POINT ( 'NONE',  ( -4.243569643749998122, -18.26903647401939779, -6.080898069690205965 ) ) ;
#11959 = CARTESIAN_POINT ( 'NONE',  ( 4.243569643750003451, -22.51708695574430763, -12.14774289770557303 ) ) ;
#11960 = AXIS2_PLACEMENT_3D ( 'NONE', #5696, #13010, #5781 ) ;
#11961 = CARTESIAN_POINT ( 'NONE',  ( 4.000000000000000888, -26.49749225125177432, -13.56086067486898372 ) ) ;
#11962 = ORIENTED_EDGE ( 'NONE', *, *, #15229, .F. ) ;
#11963 = CARTESIAN_POINT ( 'NONE',  ( 8.535862155146745067, -10.00000000000000178, 16.49127580077287902 ) ) ;
#11964 = DIRECTION ( 'NONE',  ( -0.000000000000000000, -1.000000000000000000, -0.000000000000000000 ) ) ;
#11965 = FACE_OUTER_BOUND ( 'NONE', #3317, .T. ) ;
#11966 = CARTESIAN_POINT ( 'NONE',  ( -5.330712181944245322E-15, -30.94693959492275681, -11.37234980655397010 ) ) ;
#11967 = ORIENTED_EDGE ( 'NONE', *, *, #15610, .T. ) ;
#11968 = CARTESIAN_POINT ( 'NONE',  ( 1.135272562821020070, 30.25319992234354416, -3.311245368580577164 ) ) ;
#11969 = CARTESIAN_POINT ( 'NONE',  ( 3.500000000000000444, 15.75319992234354416, 0.05647727720529520379 ) ) ;
#11970 = CARTESIAN_POINT ( 'NONE',  ( -4.243569643750000786, -22.06123700099670870, -7.225231581817909365 ) ) ;
#11971 = CARTESIAN_POINT ( 'NONE',  ( -1.497042530366477164, 25.12180007765648071, 2.161531897785062384 ) ) ;
#11972 = CARTESIAN_POINT ( 'NONE',  ( -2.733110507866328476, 14.87819992234354238, -3.862833514489096398 ) ) ;
#11973 = CARTESIAN_POINT ( 'NONE',  ( 4.730628863548789710E-15, -22.27389062868905967, -16.07191265961602511 ) ) ;
#11974 = CARTESIAN_POINT ( 'NONE',  ( 4.000000000000003553, -24.26159577562626524, -14.39398748700122077 ) ) ;
#11975 = CARTESIAN_POINT ( 'NONE',  ( -4.243569643750000786, -21.06106309010958100, -5.796835204588974833 ) ) ;
#11976 = CARTESIAN_POINT ( 'NONE',  ( 2.829195390882805583, 37.12180007765647360, 3.793023760679204770 ) ) ;
#11977 = DIRECTION ( 'NONE',  ( -1.000000000000000000, 0.000000000000000000, -0.000000000000000000 ) ) ;
#11978 = CARTESIAN_POINT ( 'NONE',  ( -1.734723475976807094E-15, 40.79999999999999716, -2.500000000000000000 ) ) ;
#11979 = ORIENTED_EDGE ( 'NONE', *, *, #11440, .T. ) ;
#11980 = ORIENTED_EDGE ( 'NONE', *, *, #7387, .F. ) ;
#11981 = EDGE_CURVE ( 'NONE', #17584, #16586, #15016, .T. ) ;
#11982 = CARTESIAN_POINT ( 'NONE',  ( 8.000000000000005329, 43.00000000000000000, 2.499999999999997780 ) ) ;
#11983 = CARTESIAN_POINT ( 'NONE',  ( 10.00000000000000000, 20.99999999999999289, -2.500000000000003109 ) ) ;
#11984 = VERTEX_POINT ( 'NONE', #1523 ) ;
#11985 = CARTESIAN_POINT ( 'NONE',  ( 2.518350579753611207, 28.12819992234355126, -0.7558219633769606149 ) ) ;
#11986 = CARTESIAN_POINT ( 'NONE',  ( 2.121784821875004390, -21.97606102313498511, -13.51082284627447017 ) ) ;
#11987 = CARTESIAN_POINT ( 'NONE',  ( 3.518350579753631191, 21.87180007765647360, 1.080741659609802285 ) ) ;
#11988 = VECTOR ( 'NONE', #11713, 1000.000000000000000 ) ;
#11989 = CARTESIAN_POINT ( 'NONE',  ( 0.000000000000000000, 0.000000000000000000, 30.00000000000000000 ) ) ;
#11990 = ADVANCED_FACE ( 'NONE', ( #15608 ), #1342, .F. ) ;
#11991 = CARTESIAN_POINT ( 'NONE',  ( 3.122678035296257093, -15.23680830283740129, -9.380745725235836829 ) ) ;
#11992 = CARTESIAN_POINT ( 'NONE',  ( -4.243569643749997233, -23.72159747208149128, -13.86796219071246306 ) ) ;
#11993 = CARTESIAN_POINT ( 'NONE',  ( 4.000000000000000000, -1.759474945355381292, 3.047500000000002540 ) ) ;
#11994 = DIRECTION ( 'NONE',  ( 0.000000000000000000, 0.000000000000000000, -1.000000000000000000 ) ) ;
#11995 = LINE ( 'NONE', #9396, #4670 ) ;
#11996 = CARTESIAN_POINT ( 'NONE',  ( -2.121784821874996396, -20.12627701590287543, -10.86905750344246435 ) ) ;
#11997 = AXIS2_PLACEMENT_3D ( 'NONE', #14302, #12627, #14210 ) ;
#11998 = EDGE_LOOP ( 'NONE', ( #4296, #1658, #3140, #1353 ) ) ;
#11999 = FACE_OUTER_BOUND ( 'NONE', #9383, .T. ) ;
#12000 = CARTESIAN_POINT ( 'NONE',  ( 0.000000000000000000, 9.254131787996968228, 30.52396275209373044 ) ) ;
#12001 = CARTESIAN_POINT ( 'NONE',  ( 2.055738996568313048, 26.99680007765647716, 1.423772053676023441 ) ) ;
#12002 = FACE_OUTER_BOUND ( 'NONE', #3971, .T. ) ;
#12003 = CARTESIAN_POINT ( 'NONE',  ( 3.481649420246370141, 29.12180007765647360, -1.193696214020541602 ) ) ;
#12004 = CARTESIAN_POINT ( 'NONE',  ( -3.999999999999997335, -24.75630545268398208, -15.10050612620724841 ) ) ;
#12005 = APPLICATION_PROTOCOL_DEFINITION ( 'draft international standard', 'automotive_design', 1998, #16747 ) ;
#12006 = CARTESIAN_POINT ( 'NONE',  ( -13.00000000000000178, 49.00000000000000000, -16.00000000000000000 ) ) ;
#12007 = VERTEX_POINT ( 'NONE', #7157 ) ;
#12008 = CARTESIAN_POINT ( 'NONE',  ( -4.243569643750004339, -24.33704482437095251, -6.203931876856584537 ) ) ;
#12009 = CARTESIAN_POINT ( 'NONE',  ( -2.115076519116362519, 17.62180007765647716, 3.012182706137107147 ) ) ;
#12010 =( BOUNDED_SURFACE ( )  B_SPLINE_SURFACE ( 3, 2, ( 
 ( #3106, #8644, #1620 ),
 ( #8736, #1716, #7352 ),
 ( #13012, #324, #14514 ),
 ( #5962, #11616, #1812 ),
 ( #7448, #13105, #6057 ),
 ( #11709, #2003, #16097 ),
 ( #10416, #3292, #511 ),
 ( #7541, #2097, #1913 ),
 ( #787, #13196, #6348 ),
 ( #17499, #16179, #4764 ),
 ( #6523, #7724, #11991 ),
 ( #14800, #8931, #3654 ),
 ( #9302, #880, #3476 ),
 ( #11898, #6247, #14894 ),
 ( #17780, #13385, #17685 ),
 ( #14979, #700, #17596 ),
 ( #12173, #4862, #12078 ),
 ( #14707, #17863, #4947 ) ),
 .UNSPECIFIED., .F., .F., .T. ) 
 B_SPLINE_SURFACE_WITH_KNOTS ( ( 4, 2, 2, 2, 2, 2, 2, 2, 4 ),
 ( 3, 3 ),
 ( 5.253488506341834174, 5.382200606446552626, 5.510912706551271967, 5.639624806655991307, 5.768336906760710647, 5.897049006865429988, 6.025761106970148440, 6.154473207074866892, 6.283185307179586232 ),
 ( 0.000000000000000000, 1.000000000000000000 ),
 .UNSPECIFIED. ) 
 GEOMETRIC_REPRESENTATION_ITEM ( )  RATIONAL_B_SPLINE_SURFACE ( (
 ( 1.000000000000000000, 0.5376207706124462860, 1.000000000000000000),
 ( 1.000000000000000000, 0.5236136374383226766, 1.000000000000000000),
 ( 1.000000000000000000, 0.5095962305068678644, 1.000000000000000000),
 ( 1.000000000000000000, 0.4818058245216391144, 1.000000000000000000),
 ( 1.000000000000000000, 0.4680310812906506301, 1.000000000000000000),
 ( 1.000000000000000000, 0.4410557726863417738, 1.000000000000000000),
 ( 1.000000000000000000, 0.4278543698619108882, 1.000000000000000000),
 ( 1.000000000000000000, 0.4024558808744606586, 1.000000000000000000),
 ( 1.000000000000000000, 0.3902583003213770385, 1.000000000000000000),
 ( 1.000000000000000000, 0.3674181228096251028, 1.000000000000000000),
 ( 1.000000000000000000, 0.3567764320979142645, 1.000000000000000000),
 ( 1.000000000000000000, 0.3377179606062171713, 1.000000000000000000),
 ( 1.000000000000000000, 0.3293051245441800390, 1.000000000000000000),
 ( 1.000000000000000000, 0.3154271731554472158, 1.000000000000000000),
 ( 1.000000000000000000, 0.3099694920613502158, 1.000000000000000000),
 ( 1.000000000000000000, 0.3026053347213686351, 1.000000000000000000),
 ( 1.000000000000000000, 0.3006987634938562692, 1.000000000000000000),
 ( 1.000000000000000000, 0.3007057995042700660, 1.000000000000000000) ) ) 
 REPRESENTATION_ITEM ( '' )  SURFACE ( )  );
#12011 = ORIENTED_EDGE ( 'NONE', *, *, #8243, .F. ) ;
#12012 = TOROIDAL_SURFACE ( 'NONE', #9353, 9.000000000000001776, 0.9999999999999991118 ) ;
#12013 = CARTESIAN_POINT ( 'NONE',  ( 1.071796769724485232, -24.85849519618256664, -4.246343115131230306 ) ) ;
#12014 = AXIS2_PLACEMENT_3D ( 'NONE', #17403, #15711, #12913 ) ;
#12015 = DIRECTION ( 'NONE',  ( -0.000000000000000000, -1.000000000000000000, -0.000000000000000000 ) ) ;
#12016 = EDGE_CURVE ( 'NONE', #10059, #14859, #8810, .T. ) ;
#12017 = DIRECTION ( 'NONE',  ( 1.000000000000000000, 0.000000000000000000, 0.000000000000000000 ) ) ;
#12018 = CARTESIAN_POINT ( 'NONE',  ( -1.734723475976807094E-15, 16.59999999999999787, -11.50000000000000178 ) ) ;
#12019 = CARTESIAN_POINT ( 'NONE',  ( 0.000000000000000000, 48.00000000000000000, 16.00000000000000000 ) ) ;
#12020 = CARTESIAN_POINT ( 'NONE',  ( -9.184850993605147944E-16, 43.00000000000000000, -2.500000000000000000 ) ) ;
#12021 = CARTESIAN_POINT ( 'NONE',  ( 4.243569643750000786, -20.67389899557263533, -5.243907574693898788 ) ) ;
#12022 = ORIENTED_EDGE ( 'NONE', *, *, #8300, .F. ) ;
#12023 = FACE_OUTER_BOUND ( 'NONE', #7860, .T. ) ;
#12024 = CARTESIAN_POINT ( 'NONE',  ( -4.000000000000004441, -25.65758508623986600, -8.335031024230250551 ) ) ;
#12025 = ORIENTED_EDGE ( 'NONE', *, *, #9598, .T. ) ;
#12026 = EDGE_LOOP ( 'NONE', ( #374, #190, #17891, #9716, #17230 ) ) ;
#12027 = CARTESIAN_POINT ( 'NONE',  ( -1.734723475976807094E-15, 43.00000000000000000, -2.500000000000000000 ) ) ;
#12028 = SURFACE_SIDE_STYLE ('',( #10642 ) ) ;
#12029 = PRESENTATION_STYLE_ASSIGNMENT (( #919 ) ) ;
#12030 = CARTESIAN_POINT ( 'NONE',  ( -3.607379964056363075, 22.25319992234354416, -2.690724712371229899 ) ) ;
#12031 = CARTESIAN_POINT ( 'NONE',  ( -3.481649420246394566, 34.62819992234354771, -1.193696214020467883 ) ) ;
#12032 = VECTOR ( 'NONE', #9307, 1000.000000000000000 ) ;
#12033 = CARTESIAN_POINT ( 'NONE',  ( -2.481649420246391902, 22.12819992234354771, -0.8687765177875723666 ) ) ;
#12034 = EDGE_LOOP ( 'NONE', ( #18128, #15834, #6048 ) ) ;
#12035 = CARTESIAN_POINT ( 'NONE',  ( 2.733110507866247652, 16.37180007765647716, -3.862833514489153686 ) ) ;
#12036 = CARTESIAN_POINT ( 'NONE',  ( 4.713407268011036227E-15, -18.19707658806250805, -9.759274404511186773 ) ) ;
#12037 = ORIENTED_EDGE ( 'NONE', *, *, #6811, .T. ) ;
#12038 = CARTESIAN_POINT ( 'NONE',  ( -5.577813053751546416E-15, -29.25788163498686245, -10.52931808859795559 ) ) ;
#12039 = CARTESIAN_POINT ( 'NONE',  ( 2.115076519116362963, 36.37180007765648782, -3.012182706137107147 ) ) ;
#12040 = EDGE_CURVE ( 'NONE', #4710, #9347, #12819, .T. ) ;
#12041 = DIRECTION ( 'NONE',  ( 0.000000000000000000, 0.000000000000000000, 1.000000000000000000 ) ) ;
#12042 = EDGE_CURVE ( 'NONE', #196, #15374, #4206, .T. ) ;
#12043 = CARTESIAN_POINT ( 'NONE',  ( 2.121784821874994176, -23.69506935700625050, -3.151350836941627875 ) ) ;
#12044 = EDGE_CURVE ( 'NONE', #11008, #4334, #2328, .T. ) ;
#12045 = AXIS2_PLACEMENT_3D ( 'NONE', #3641, #9288, #11977 ) ;
#12046 = CARTESIAN_POINT ( 'NONE',  ( -5.330712181944245322E-15, -27.84962683862713106, -6.948928767393398154 ) ) ;
#12047 = CARTESIAN_POINT ( 'NONE',  ( -3.500000000000000444, 15.49680007765647893, 0.05647727720536901974 ) ) ;
#12048 = VERTEX_POINT ( 'NONE', #9765 ) ;
#12049 = CARTESIAN_POINT ( 'NONE',  ( -4.000000000000000888, -19.85117529432912775, -4.068936360663492735 ) ) ;
#12050 = FILL_AREA_STYLE_COLOUR ( '', #9850 ) ;
#12051 = CARTESIAN_POINT ( 'NONE',  ( -2.121784821875005722, -29.70686738051060161, -11.73708820114566009 ) ) ;
#12052 = VERTEX_POINT ( 'NONE', #5597 ) ;
#12053 = CARTESIAN_POINT ( 'NONE',  ( 3.518350579753605434, 30.62819992234353705, -1.080741659609877114 ) ) ;
#12054 = CARTESIAN_POINT ( 'NONE',  ( -1.734723475976807094E-15, 31.99999999999999289, -11.50000000000000178 ) ) ;
#12055 = CARTESIAN_POINT ( 'NONE',  ( -2.121784821874996396, -18.31951124139709464, -8.288728563932130200 ) ) ;
#12056 = CARTESIAN_POINT ( 'NONE',  ( -0.7188294034286043521, 19.99680007765648071, 2.395093729190366005 ) ) ;
#12057 = CARTESIAN_POINT ( 'NONE',  ( -4.499999999999999112, 17.00319992234354416, -0.05647727720528529505 ) ) ;
#12058 = AXIS2_PLACEMENT_3D ( 'NONE', #12655, #8389, #5792 ) ;
#12059 = CARTESIAN_POINT ( 'NONE',  ( -5.279047395330986450E-15, -29.50666528769278685, -9.805769334647276736 ) ) ;
#12060 = CARTESIAN_POINT ( 'NONE',  ( -4.243569643750000786, -20.80295369375161130, -5.428216784658927985 ) ) ;
#12061 = CARTESIAN_POINT ( 'NONE',  ( 2.798362969681366330, 16.49680007765647716, -2.102939460078824929 ) ) ;
#12062 = DIRECTION ( 'NONE',  ( -0.000000000000000000, -0.5735764363510414965, -0.8191520442889950182 ) ) ;
#12063 = CARTESIAN_POINT ( 'NONE',  ( 3.082316921986471225, -29.06618978543598786, -12.78463801463987437 ) ) ;
#12064 = PRESENTATION_LAYER_ASSIGNMENT (  '', '', ( #9693 ) ) ;
#12065 = DIRECTION ( 'NONE',  ( -0.000000000000000000, -0.5735764363510414965, -0.8191520442889950182 ) ) ;
#12066 = ORIENTED_EDGE ( 'NONE', *, *, #6323, .T. ) ;
#12067 = ORIENTED_EDGE ( 'NONE', *, *, #7161, .T. ) ;
#12068 = DIRECTION ( 'NONE',  ( -0.000000000000000000, -0.5735764363510414965, -0.8191520442889950182 ) ) ;
#12070 = ADVANCED_FACE ( 'NONE', ( #12547 ), #10294, .F. ) ;
#12069 = LINE ( 'NONE', #9020, #16589 ) ;
#12071 = CARTESIAN_POINT ( 'NONE',  ( -3.604268994871580478, -29.04518628171981476, -12.79934482627075276 ) ) ;
#12072 = ORIENTED_EDGE ( 'NONE', *, *, #2587, .T. ) ;
#12073 = CARTESIAN_POINT ( 'NONE',  ( 1.989345975306457071, 28.50319992234355126, 1.515154207786300500 ) ) ;
#12074 = SURFACE_STYLE_FILL_AREA ( #7814 ) ;
#12075 = CARTESIAN_POINT ( 'NONE',  ( -4.243569643750005227, -27.91831269883777011, -11.31851245338599377 ) ) ;
#12076 = CARTESIAN_POINT ( 'NONE',  ( 2.798362969681366330, 23.99680007765647716, -2.102939460078824929 ) ) ;
#12077 = CARTESIAN_POINT ( 'NONE',  ( 0.000000000000000000, 9.254131787996968228, 30.52396275209373044 ) ) ;
#12078 = CARTESIAN_POINT ( 'NONE',  ( 0.3217809247882234547, -15.45745613286858244, -10.86990606519723279 ) ) ;
#12079 = PRODUCT_DEFINITION_SHAPE ( 'NONE', 'NONE',  #18378 ) ;
#12080 = TOROIDAL_SURFACE ( 'NONE', #4087, 9.000000000000001776, 0.9999999999999991118 ) ;
#12081 = CARTESIAN_POINT ( 'NONE',  ( -4.243569643750005227, -27.17624818430860856, -10.25873449608710608 ) ) ;
#12082 = TOROIDAL_SURFACE ( 'NONE', #17453, 9.000000000000001776, 0.9999999999999991118 ) ;
#12083 = DIRECTION ( 'NONE',  ( 0.000000000000000000, 1.000000000000000000, -1.478898702612462246E-15 ) ) ;
#12084 = EDGE_CURVE ( 'NONE', #16667, #7464, #11476, .T. ) ;
#12085 = DIRECTION ( 'NONE',  ( 0.000000000000000000, 0.000000000000000000, 1.000000000000000000 ) ) ;
#12086 = ADVANCED_FACE ( 'NONE', ( #1436 ), #12082, .T. ) ;
#12087 = FACE_BOUND ( 'NONE', #10443, .T. ) ;
#12088 = CARTESIAN_POINT ( 'NONE',  ( -4.243569643750005227, -25.59532813161604636, -8.000946674015564142 ) ) ;
#12089 = ORIENTED_EDGE ( 'NONE', *, *, #10561, .T. ) ;
#12090 = CARTESIAN_POINT ( 'NONE',  ( 4.898587196589413815E-16, 2.700915433685006750, 35.11257424290206330 ) ) ;
#12091 = CARTESIAN_POINT ( 'NONE',  ( -8.500000000000010658, 15.00000000000000000, 18.29999999999999005 ) ) ;
#12092 = VECTOR ( 'NONE', #3613, 1000.000000000000227 ) ;
#12093 = CARTESIAN_POINT ( 'NONE',  ( 0.8262555684461332373, 32.24680007765648071, 2.360188852285403982 ) ) ;
#12094 = AXIS2_PLACEMENT_3D ( 'NONE', #3162, #8799, #3258 ) ;
#12095 = ORIENTED_EDGE ( 'NONE', *, *, #6327, .F. ) ;
#12096 = CARTESIAN_POINT ( 'NONE',  ( -2.798362969681365886, 30.24680007765648071, 2.102939460078824929 ) ) ;
#12097 = LINE ( 'NONE', #10709, #5113 ) ;
#12098 = APPLICATION_PROTOCOL_DEFINITION ( 'draft international standard', 'automotive_design', 1998, #3111 ) ;
#12099 = DIRECTION ( 'NONE',  ( -0.9454169814551715012, 0.000000000000000000, 0.3258630558627224061 ) ) ;
#12100 = ORIENTED_EDGE ( 'NONE', *, *, #16828, .F. ) ;
#12101 = CARTESIAN_POINT ( 'NONE',  ( 2.121784821874994176, -25.79220820241474854, -6.146375498873266174 ) ) ;
#12102 = CARTESIAN_POINT ( 'NONE',  ( 2.864755990943265829, 21.99680007765647716, 2.011557305968487697 ) ) ;
#12103 = VERTEX_POINT ( 'NONE', #5773 ) ;
#12104 = AXIS2_PLACEMENT_3D ( 'NONE', #11929, #7932, #5158 ) ;
#12105 = CARTESIAN_POINT ( 'NONE',  ( -9.000000000000001776, 29.79999999999999716, 2.499999999999998224 ) ) ;
#12106 = CIRCLE ( 'NONE', #18070, 0.3999999999999991895 ) ;
#12107 = CARTESIAN_POINT ( 'NONE',  ( 4.000000000000000000, 3.518949890710770134, -4.119968255444916849E-15 ) ) ;
#12108 = DIRECTION ( 'NONE',  ( -3.469446951953613696E-16, -0.000000000000000000, -1.000000000000000000 ) ) ;
#12109 = CARTESIAN_POINT ( 'NONE',  ( 7.471583913895156748, -13.11946146044265227, 4.276027703312072603 ) ) ;
#12110 = ADVANCED_FACE ( 'NONE', ( #17021 ), #4292, .F. ) ;
#12111 = CARTESIAN_POINT ( 'NONE',  ( 3.999999999999996447, -26.53945885642465186, -9.594477291317806689 ) ) ;
#12112 = CARTESIAN_POINT ( 'NONE',  ( 4.243569643749996345, -22.18613318805455847, -3.132111710772846891 ) ) ;
#12113 = ORIENTED_EDGE ( 'NONE', *, *, #1917, .F. ) ;
#12114 = CARTESIAN_POINT ( 'NONE',  ( 8.000000000000001776, 34.19999999999999574, -2.500000000000002220 ) ) ;
#12115 = CARTESIAN_POINT ( 'NONE',  ( 4.000000000000003553, -21.22881036912508179, -10.06272105382992521 ) ) ;
#12116 = AXIS2_PLACEMENT_3D ( 'NONE', #3485, #16289, #9132 ) ;
#12117 = CARTESIAN_POINT ( 'NONE',  ( 2.798362969681366330, 31.49680007765647716, -2.102939460078824929 ) ) ;
#12118 = ORIENTED_EDGE ( 'NONE', *, *, #10971, .T. ) ;
#12119 = ORIENTED_EDGE ( 'NONE', *, *, #18203, .F. ) ;
#12120 = LINE ( 'NONE', #13237, #11918 ) ;
#12121 = AXIS2_PLACEMENT_3D ( 'NONE', #18190, #8494, #17059 ) ;
#12122 = CARTESIAN_POINT ( 'NONE',  ( 1.336863392178569754, 31.25319992234354416, 4.297206761780648421 ) ) ;
#12123 = CARTESIAN_POINT ( 'NONE',  ( -1.027846397803611866, 35.00319992234354771, -3.346150245485499219 ) ) ;
#12124 = CARTESIAN_POINT ( 'NONE',  ( 1.989345975306457071, 26.00319992234354771, 1.515154207786300500 ) ) ;
#12125 = ORIENTED_EDGE ( 'NONE', *, *, #8168, .T. ) ;
#12126 = CARTESIAN_POINT ( 'NONE',  ( -4.518350579753602325, 39.37819992234354771, 1.405661355842794391 ) ) ;
#12127 = CARTESIAN_POINT ( 'NONE',  ( -4.000000000000004441, -22.75385437650777476, -4.188073799010446407 ) ) ;
#12128 = ORIENTED_EDGE ( 'NONE', *, *, #2527, .F. ) ;
#12129 = DIRECTION ( 'NONE',  ( 0.000000000000000000, 0.000000000000000000, -1.000000000000000000 ) ) ;
#12130 = CARTESIAN_POINT ( 'NONE',  ( 3.481649420246369697, 36.62180007765648071, -1.193696214020541824 ) ) ;
#12131 = CARTESIAN_POINT ( 'NONE',  ( -8.500000000000005329, 10.00000000000000000, 18.49999999999999645 ) ) ;
#12132 = CIRCLE ( 'NONE', #7096, 8.000000000000001776 ) ;
#12133 = CARTESIAN_POINT ( 'NONE',  ( -4.243569643750004339, -22.49801537532042417, -3.577525634854993086 ) ) ;
#12134 = CARTESIAN_POINT ( 'NONE',  ( 4.730628863548789710E-15, -19.69279666510938043, -12.38572846031554953 ) ) ;
#12135 = CARTESIAN_POINT ( 'NONE',  ( -0.4744323633459381351, -30.28477276999926460, -12.01443746324198258 ) ) ;
#12136 = EDGE_LOOP ( 'NONE', ( #1242, #4915, #2325, #10946 ) ) ;
#12137 = CARTESIAN_POINT ( 'NONE',  ( 3.544496300715735071, -10.00000000000000178, 23.01862375599375099 ) ) ;
#12138 = SURFACE_STYLE_FILL_AREA ( #17745 ) ;
#12139 = CARTESIAN_POINT ( 'NONE',  ( 4.299564228933482956E-15, -19.47829782620029704, -10.51019933028069708 ) ) ;
#12140 = CARTESIAN_POINT ( 'NONE',  ( 4.730628863548789710E-15, -22.53200002504703647, -16.44053107954607640 ) ) ;
#12141 = VERTEX_POINT ( 'NONE', #13944 ) ;
#12142 = CARTESIAN_POINT ( 'NONE',  ( 2.211161402132839626, 32.87819992234354771, -2.942372952327218183 ) ) ;
#12143 = DIRECTION ( 'NONE',  ( 0.000000000000000000, 0.000000000000000000, 1.000000000000000000 ) ) ;
#12144 = CARTESIAN_POINT ( 'NONE',  ( -5.330712181944245322E-15, -24.20383161507082193, -1.742193585881474771 ) ) ;
#12145 = CARTESIAN_POINT ( 'NONE',  ( -2.518350579753628526, 23.12180007765647005, -0.7558219633769075463 ) ) ;
#12146 = EDGE_CURVE ( 'NONE', #9517, #13037, #6171, .T. ) ;
#12147 = AXIS2_PLACEMENT_3D ( 'NONE', #6137, #17484, #17846 ) ;
#12148 = CARTESIAN_POINT ( 'NONE',  ( 4.499999999999999112, 18.25319992234354771, 0.05647727720528474687 ) ) ;
#12149 = ADVANCED_FACE ( 'NONE', ( #6803 ), #13276, .T. ) ;
#12150 = CARTESIAN_POINT ( 'NONE',  ( -2.000000000000005773, -28.32418970114301260, -10.13017813623426733 ) ) ;
#12151 = ORIENTED_EDGE ( 'NONE', *, *, #16822, .F. ) ;
#12152 = EDGE_CURVE ( 'NONE', #1548, #7899, #2346, .T. ) ;
#12153 = CARTESIAN_POINT ( 'NONE',  ( 2.121784821874994176, -24.50166122062490359, -4.303283399223027494 ) ) ;
#12154 = CARTESIAN_POINT ( 'NONE',  ( -1.336863392178478716, 39.99680007765647360, 4.297206761780677731 ) ) ;
#12155 = EDGE_CURVE ( 'NONE', #16507, #6514, #12372, .T. ) ;
#12156 = CYLINDRICAL_SURFACE ( 'NONE', #6142, 3.799999999999999378 ) ;
#12157 = AXIS2_PLACEMENT_3D ( 'NONE', #17716, #4983, #3771 ) ;
#12158 = CARTESIAN_POINT ( 'NONE',  ( 8.000000000000001776, 40.79999999999999716, -2.500000000000002220 ) ) ;
#12159 = CARTESIAN_POINT ( 'NONE',  ( 4.000000000000003553, -20.71259157640914594, -9.325484213969829739 ) ) ;
#12160 = ORIENTED_EDGE ( 'NONE', *, *, #2798, .F. ) ;
#12161 = ORIENTED_EDGE ( 'NONE', *, *, #11937, .F. ) ;
#12162 = CARTESIAN_POINT ( 'NONE',  ( -0.05938372350927861171, 18.62180007765647005, -3.680117784833935701 ) ) ;
#12163 = EDGE_CURVE ( 'NONE', #3667, #723, #10908, .T. ) ;
#12164 = CARTESIAN_POINT ( 'NONE',  ( 4.000000000000000888, -26.75560164760974047, -13.92947909479903146 ) ) ;
#12165 = CARTESIAN_POINT ( 'NONE',  ( 8.000000000000001776, 27.59999999999999432, -2.500000000000002220 ) ) ;
#12166 = ORIENTED_EDGE ( 'NONE', *, *, #12816, .F. ) ;
#12167 = CARTESIAN_POINT ( 'NONE',  ( -0.05938372350921170689, 28.87819992234354416, 2.628655560595669183 ) ) ;
#12168 =( LENGTH_UNIT ( ) NAMED_UNIT ( * ) SI_UNIT ( .MILLI., .METRE. ) );
#12169 = CARTESIAN_POINT ( 'NONE',  ( 4.243569643750003451, -22.48482328119956009, -12.10166559521431573 ) ) ;
#12170 = CARTESIAN_POINT ( 'NONE',  ( -2.115076519116362519, 20.12180007765648071, 3.012182706137107147 ) ) ;
#12171 = PRODUCT_DEFINITION ( 'UNKNOWN', '', #16965, #6916 ) ;
#12172 = DIRECTION ( 'NONE',  ( -0.000000000000000000, -0.5735764363510414965, -0.8191520442889950182 ) ) ;
#12173 = CARTESIAN_POINT ( 'NONE',  ( 0.4504932947034594459, -10.00000000000000178, -12.59063537424963997 ) ) ;
#12174 = CIRCLE ( 'NONE', #5154, 0.9999999999999991118 ) ;
#12175 =( GEOMETRIC_REPRESENTATION_CONTEXT ( 3 ) GLOBAL_UNCERTAINTY_ASSIGNED_CONTEXT ( ( #9551 ) ) GLOBAL_UNIT_ASSIGNED_CONTEXT ( ( #12168, #2186, #505 ) ) REPRESENTATION_CONTEXT ( 'NONE', 'WORKASPACE' ) );
#12176 = CARTESIAN_POINT ( 'NONE',  ( 4.243569643750000786, -25.57797752637403832, -12.24765755336480666 ) ) ;
#12177 = DIRECTION ( 'NONE',  ( 0.000000000000000000, -1.000000000000000000, 0.000000000000000000 ) ) ;
#12178 = CARTESIAN_POINT ( 'NONE',  ( -2.733110507866247652, 25.12180007765648071, 3.862833514489154574 ) ) ;
#12179 = DIRECTION ( 'NONE',  ( -1.000000000000000000, 0.000000000000000000, 0.000000000000000000 ) ) ;
#12180 = DIRECTION ( 'NONE',  ( -0.000000000000000000, -0.5735764363510414965, -0.8191520442889950182 ) ) ;
#12181 = CARTESIAN_POINT ( 'NONE',  ( -4.243569643749997233, -20.59202104124112154, -9.398463849060638253 ) ) ;
#12182 = EDGE_LOOP ( 'NONE', ( #8203, #15386, #371, #18270 ) ) ;
#12183 = DIRECTION ( 'NONE',  ( -3.469446951953613696E-16, -0.000000000000000000, -1.000000000000000000 ) ) ;
#12184 = DIRECTION ( 'NONE',  ( 1.000000000000000000, 0.000000000000000000, -0.000000000000000000 ) ) ;
#12186 = DIRECTION ( 'NONE',  ( 0.000000000000000000, 1.000000000000000000, 0.000000000000000000 ) ) ;
#12185 = STYLED_ITEM ( 'NONE', ( #4436 ), #9153 ) ;
#12187 = CARTESIAN_POINT ( 'NONE',  ( 1.593127413382998903, 29.62180007765647716, 2.091722143975139669 ) ) ;
#12188 = CARTESIAN_POINT ( 'NONE',  ( 3.250762944584260072, -21.87258937905581746, -2.200190645090608577 ) ) ;
#12189 = CARTESIAN_POINT ( 'NONE',  ( 2.798362969681366330, 28.99680007765647716, -2.102939460078824929 ) ) ;
#12190 = CYLINDRICAL_SURFACE ( 'NONE', #686, 0.9999999999999991118 ) ;
#12191 = APPLICATION_PROTOCOL_DEFINITION ( 'draft international standard', 'automotive_design', 1998, #6987 ) ;
#12192 = ORIENTED_EDGE ( 'NONE', *, *, #4453, .T. ) ;
#12193 = VECTOR ( 'NONE', #10841, 1000.000000000000000 ) ;
#12194 = CARTESIAN_POINT ( 'NONE',  ( 4.243569643749997233, -24.76722715163424127, -6.818295910073324251 ) ) ;
#12195 = CARTESIAN_POINT ( 'NONE',  ( -0.05938372350927861171, 26.12180007765647005, -3.680117784833935701 ) ) ;
#12196 = ORIENTED_EDGE ( 'NONE', *, *, #6323, .F. ) ;
#12197 = STYLED_ITEM ( 'NONE', ( #5356 ), #10928 ) ;
#12198 = CARTESIAN_POINT ( 'NONE',  ( 0.000000000000000000, -1.443375672974064328, 1.278502688459867223E-18 ) ) ;
#12199 = CARTESIAN_POINT ( 'NONE',  ( 2.399999999999999911, 0.000000000000000000, 0.000000000000000000 ) ) ;
#12200 = DIRECTION ( 'NONE',  ( -0.000000000000000000, -1.000000000000000000, -0.000000000000000000 ) ) ;
#12201 = CARTESIAN_POINT ( 'NONE',  ( 9.996570547186806266, -9.916659267309226422, 4.908050019500779015 ) ) ;
#12202 = CARTESIAN_POINT ( 'NONE',  ( -3.706921591972381904E-14, -17.67153205169451624, -7.929870390770359379 ) ) ;
#12203 = CARTESIAN_POINT ( 'NONE',  ( -2.121784821874996396, -16.80311853779403108, -6.123095346843099307 ) ) ;
#12204 = ORIENTED_EDGE ( 'NONE', *, *, #2716, .T. ) ;
#12205 = CARTESIAN_POINT ( 'NONE',  ( -4.648177544792955347E-16, -30.03220982406077155, -11.63517334838810058 ) ) ;
#12206 = VECTOR ( 'NONE', #2500, 1000.000000000000000 ) ;
#12207 = CARTESIAN_POINT ( 'NONE',  ( -3.999999999999997335, -21.91710209274632604, -11.04570350697672332 ) ) ;
#12208 = CIRCLE ( 'NONE', #6592, 4.000000000000000000 ) ;
#12209 = CARTESIAN_POINT ( 'NONE',  ( -2.798362969681365886, 27.74680007765648071, 2.102939460078824929 ) ) ;
#12210 = EDGE_LOOP ( 'NONE', ( #12684, #292, #11095, #12389 ) ) ;
#12211 = ORIENTED_EDGE ( 'NONE', *, *, #10806, .T. ) ;
#12212 = CARTESIAN_POINT ( 'NONE',  ( 1.071796769724487675, -29.56899168042044224, -10.97362927986136860 ) ) ;
#12213 = CARTESIAN_POINT ( 'NONE',  ( 1.444289557195957086, 35.25319992234354771, -4.262301884875733471 ) ) ;
#12214 = DIRECTION ( 'NONE',  ( -0.000000000000000000, 1.000000000000000000, -0.000000000000000000 ) ) ;
#12215 = CARTESIAN_POINT ( 'NONE',  ( 0.05938372350921204690, 30.12819992234354416, -2.628655560595669183 ) ) ;
#12216 = ORIENTED_EDGE ( 'NONE', *, *, #9827, .T. ) ;
#12217 = CARTESIAN_POINT ( 'NONE',  ( 3.607379964056306676, 28.99680007765648071, -2.690724712371305838 ) ) ;
#12218 = ADVANCED_FACE ( 'NONE', ( #17486 ), #7616, .T. ) ;
#12219 = CARTESIAN_POINT ( 'NONE',  ( 1.999999999999994449, -23.11898354125731458, -2.696373334311634284 ) ) ;
#12220 = ORIENTED_EDGE ( 'NONE', *, *, #4671, .F. ) ;
#12221 = TOROIDAL_SURFACE ( 'NONE', #4232, 9.000000000000001776, 0.9999999999999991118 ) ;
#12222 = DIRECTION ( 'NONE',  ( 1.000000000000000000, 0.000000000000000000, 0.000000000000000000 ) ) ;
#12223 = TOROIDAL_SURFACE ( 'NONE', #17298, 6.099999999999999645, 0.4000000000000000222 ) ;
#12224 = LINE ( 'NONE', #7779, #12092 ) ;
#12225 = CARTESIAN_POINT ( 'NONE',  ( 0.000000000000000000, 3.000000000000000000, 2.499999999999999556 ) ) ;
#12226 = CARTESIAN_POINT ( 'NONE',  ( 4.730628863548789710E-15, -16.04700144155307129, -7.178993278803623035 ) ) ;
#12227 = CARTESIAN_POINT ( 'NONE',  ( -4.243569643749997233, -21.65672230121773723, -10.91901483127208294 ) ) ;
#12228 = FACE_OUTER_BOUND ( 'NONE', #9832, .T. ) ;
#12229 = ORIENTED_EDGE ( 'NONE', *, *, #4651, .T. ) ;
#12230 = CARTESIAN_POINT ( 'NONE',  ( 0.000000000000000000, 2.449293598294706414E-16, -2.000000000000000000 ) ) ;
#12231 = CARTESIAN_POINT ( 'NONE',  ( 1.027846397803542144, 16.24680007765647716, -3.346150245485522312 ) ) ;
#12232 = CIRCLE ( 'NONE', #8986, 0.1999999999999987899 ) ;
#12233 = CARTESIAN_POINT ( 'NONE',  ( 3.579096709490575479E-14, -25.90245948233327056, -5.737278629507336802 ) ) ;
#12234 = CARTESIAN_POINT ( 'NONE',  ( 4.730628863548789710E-15, -23.04821881776296877, -17.17776791940616832 ) ) ;
#12235 = ORIENTED_EDGE ( 'NONE', *, *, #8304, .F. ) ;
#12236 = CARTESIAN_POINT ( 'NONE',  ( 2.211161402132839626, 37.87819992234352640, -2.942372952327218183 ) ) ;
#12237 = CARTESIAN_POINT ( 'NONE',  ( -4.243569643749997233, -18.52714587037736393, -6.449516489620252813 ) ) ;
#12238 = CARTESIAN_POINT ( 'NONE',  ( 1.497042530366477164, 31.37180007765648426, -2.161531897785062384 ) ) ;
#12239 = CARTESIAN_POINT ( 'NONE',  ( 1.444289557195957086, 27.75319992234354416, -4.262301884875733471 ) ) ;
#12240 = CARTESIAN_POINT ( 'NONE',  ( -5.279047395330986450E-15, -29.24855589133481715, -9.437150914717227224 ) ) ;
#12241 = ORIENTED_EDGE ( 'NONE', *, *, #9556, .T. ) ;
#12242 = CARTESIAN_POINT ( 'NONE',  ( 2.121784821874994176, -22.95300484247709250, -2.091572879642740634 ) ) ;
#12243 = CARTESIAN_POINT ( 'NONE',  ( 0.05938372350929014415, 39.87180007765647360, 4.731580009072201776 ) ) ;
#12244 = CARTESIAN_POINT ( 'NONE',  ( 13.00000000000000178, 48.00000000000000000, -16.00000000000000000 ) ) ;
#12245 = AXIS2_PLACEMENT_3D ( 'NONE', #6795, #9576, #878 ) ;
#12246 = CARTESIAN_POINT ( 'NONE',  ( -2.121784821875005722, -27.09350974238616416, -8.004826699353927211 ) ) ;
#12247 = FACE_OUTER_BOUND ( 'NONE', #13076, .T. ) ;
#12248 = ADVANCED_FACE ( 'NONE', ( #408 ), #10117, .F. ) ;
#12249 = LINE ( 'NONE', #11045, #9484 ) ;
#12250 = ADVANCED_FACE ( 'NONE', ( #1705 ), #17583, .F. ) ;
#12251 = FACE_OUTER_BOUND ( 'NONE', #9323, .T. ) ;
#12252 = ORIENTED_EDGE ( 'NONE', *, *, #18191, .T. ) ;
#12253 = VERTEX_POINT ( 'NONE', #7244 ) ;
#12254 = CARTESIAN_POINT ( 'NONE',  ( 3.481649420246369697, 19.12180007765648071, -1.193696214020541824 ) ) ;
#12255 = CARTESIAN_POINT ( 'NONE',  ( 4.299564228933482956E-15, -18.70396963712639504, -9.404344070490550322 ) ) ;
#12256 = CARTESIAN_POINT ( 'NONE',  ( 1.999999999999994449, -28.79739026113263023, -10.80597857277268403 ) ) ;
#12257 = ORIENTED_EDGE ( 'NONE', *, *, #11135, .T. ) ;
#12258 = CARTESIAN_POINT ( 'NONE',  ( -0.7188294034286550893, 35.00319992234354771, -2.395093729190349130 ) ) ;
#12259 = CARTESIAN_POINT ( 'NONE',  ( -2.121784821874996396, -21.67493339405068653, -13.08076802302275077 ) ) ;
#12260 = CARTESIAN_POINT ( 'NONE',  ( -2.864755990943265829, 30.74680007765647716, -2.011557305968488141 ) ) ;
#12261 = PRODUCT_DEFINITION_SHAPE ( 'NONE', 'NONE',  #5599 ) ;
#12262 = EDGE_CURVE ( 'NONE', #4478, #13882, #3000, .T. ) ;
#12263 = CARTESIAN_POINT ( 'NONE',  ( 2.864755990943222308, 15.50319992234354416, -2.011557305968548093 ) ) ;
#12264 = CARTESIAN_POINT ( 'NONE',  ( 0.000000000000000000, 5.977523610840987267, 32.81826849749789687 ) ) ;
#12265 = CARTESIAN_POINT ( 'NONE',  ( -4.000000000000002665, 2.343145750507628300, -2.343145750507621194 ) ) ;
#12266 = CARTESIAN_POINT ( 'NONE',  ( -2.121784821875005722, -27.64199220964684756, -8.788140841705278206 ) ) ;
#12267 = DIRECTION ( 'NONE',  ( -0.000000000000000000, -0.5735764363510414965, -0.8191520442889950182 ) ) ;
#12268 = CARTESIAN_POINT ( 'NONE',  ( 2.829195390882805583, 27.12180007765647716, 3.793023760679204770 ) ) ;
#12269 = DIRECTION ( 'NONE',  ( 3.469446951953612217E-16, -0.000000000000000000, 1.000000000000000000 ) ) ;
#12270 = EDGE_CURVE ( 'NONE', #7005, #17537, #14164, .T. ) ;
#12271 = DIRECTION ( 'NONE',  ( -0.000000000000000000, -1.000000000000000000, -0.000000000000000000 ) ) ;
#12272 = CARTESIAN_POINT ( 'NONE',  ( -5.330712181944245322E-15, -26.52681618229254212, -5.059759365251903951 ) ) ;
#12273 = EDGE_LOOP ( 'NONE', ( #14865, #8762, #7808, #7474 ) ) ;
#12274 = DIRECTION ( 'NONE',  ( 0.000000000000000000, -1.000000000000000000, 0.000000000000000000 ) ) ;
#12275 = LINE ( 'NONE', #10359, #6451 ) ;
#12276 = CARTESIAN_POINT ( 'NONE',  ( -2.481649420246374138, 35.37180007765647360, 0.8687765177876256573 ) ) ;
#12277 = DIRECTION ( 'NONE',  ( -1.000000000000000000, 0.000000000000000000, 4.336808689942021680E-16 ) ) ;
#12278 = CARTESIAN_POINT ( 'NONE',  ( -1.027846397803541700, 32.49680007765648071, 3.346150245485522312 ) ) ;
#12279 = CARTESIAN_POINT ( 'NONE',  ( -1.071796769724496334, -23.33289221947241998, -2.067556264862776771 ) ) ;
#12280 = SHAPE_DEFINITION_REPRESENTATION ( #12261, #10877 ) ;
#12281 = CARTESIAN_POINT ( 'NONE',  ( -3.636013921692167639, 15.00000000000000178, -1.612974510979999332 ) ) ;
#12282 =( BOUNDED_SURFACE ( )  B_SPLINE_SURFACE ( 3, 2, ( 
 ( #15259, #5596, #2555 ),
 ( #8186, #1253, #4202 ),
 ( #13851, #11063, #1158 ),
 ( #9667, #13942, #6887 ),
 ( #1340, #9851, #15526 ),
 ( #7242, #8629, #1702 ),
 ( #12997, #4377, #119 ),
 ( #211, #14308, #7151 ),
 ( #4751, #14593, #16078 ),
 ( #5950, #495, #1609 ),
 ( #14396, #6135, #5771 ),
 ( #17299, #10403, #11602 ),
 ( #17385, #4564, #10204 ),
 ( #3280, #11412, #6044 ),
 ( #15886, #4472, #11506 ),
 ( #1521, #3181, #15698 ),
 ( #3089, #308, #8915 ),
 ( #11788, #7338, #12817 ) ),
 .UNSPECIFIED., .F., .F., .T. ) 
 B_SPLINE_SURFACE_WITH_KNOTS ( ( 4, 2, 2, 2, 2, 2, 2, 2, 4 ),
 ( 3, 3 ),
 ( 0.000000000000000000, 0.1287121001047187574, 0.2574242002094375148, 0.3861363003141562444, 0.5148484004188750296, 0.6435605005235938147, 0.7722726006283124889, 0.9009847007330312740, 1.029696800837750059 ),
 ( 0.000000000000000000, 1.000000000000000000 ),
 .UNSPECIFIED. ) 
 GEOMETRIC_REPRESENTATION_ITEM ( )  RATIONAL_B_SPLINE_SURFACE ( (
 ( 1.000000000000000000, 0.3007057995042700660, 1.000000000000000000),
 ( 1.000000000000000000, 0.3006987634935809339, 1.000000000000000000),
 ( 1.000000000000000000, 0.3026053347217343426, 1.000000000000000000),
 ( 1.000000000000000000, 0.3099694920609858961, 1.000000000000000000),
 ( 1.000000000000000000, 0.3154271731552417135, 1.000000000000000000),
 ( 1.000000000000000000, 0.3293051245443847641, 1.000000000000000000),
 ( 1.000000000000000000, 0.3377179606062847839, 1.000000000000000000),
 ( 1.000000000000000000, 0.3567764320978462078, 1.000000000000000000),
 ( 1.000000000000000000, 0.3674181228096374263, 1.000000000000000000),
 ( 1.000000000000000000, 0.3902583003213647150, 1.000000000000000000),
 ( 1.000000000000000000, 0.4024558808744609362, 1.000000000000000000),
 ( 1.000000000000000000, 0.4278543698619110547, 1.000000000000000000),
 ( 1.000000000000000000, 0.4410557726863888472, 1.000000000000000000),
 ( 1.000000000000000000, 0.4680310812906007811, 1.000000000000000000),
 ( 1.000000000000000000, 0.4818058245216468860, 1.000000000000000000),
 ( 1.000000000000000000, 0.5095962305068602038, 1.000000000000000000),
 ( 1.000000000000000000, 0.5236136374383265624, 1.000000000000000000),
 ( 1.000000000000000000, 0.5376207706124457308, 1.000000000000000000) ) ) 
 REPRESENTATION_ITEM ( '' )  SURFACE ( )  );
#12283 = ORIENTED_EDGE ( 'NONE', *, *, #14075, .F. ) ;
#12284 = CARTESIAN_POINT ( 'NONE',  ( -4.243569643750000786, -21.57728188282551685, -6.534072044449069416 ) ) ;
#12285 = CARTESIAN_POINT ( 'NONE',  ( -3.481649420246369697, 22.87180007765647360, 1.193696214020542490 ) ) ;
#12286 = ORIENTED_EDGE ( 'NONE', *, *, #15618, .T. ) ;
#12287 = CARTESIAN_POINT ( 'NONE',  ( 1.071796769724476128, -18.45738694148725401, -9.052187485216423468 ) ) ;
#12288 = EDGE_CURVE ( 'NONE', #8695, #1204, #9123, .T. ) ;
#12289 = CARTESIAN_POINT ( 'NONE',  ( 4.243569643750000786, -26.83626083361913217, -14.04467235052378804 ) ) ;
#12290 = CARTESIAN_POINT ( 'NONE',  ( -1.734723475976807094E-15, 29.79999999999999716, -10.50000000000000178 ) ) ;
#12291 = CARTESIAN_POINT ( 'NONE',  ( 4.968999162825121552, -10.12416982780653463, -1.719962025120755023 ) ) ;
#12292 = CARTESIAN_POINT ( 'NONE',  ( -4.000000000000000888, -21.72246841862934730, -6.741419906163105047 ) ) ;
#12293 = CARTESIAN_POINT ( 'NONE',  ( -5.330712181944245322E-15, -29.88223833494613402, -9.851798824342527183 ) ) ;
#12294 = ORIENTED_EDGE ( 'NONE', *, *, #1019, .T. ) ;
#12295 = CARTESIAN_POINT ( 'NONE',  ( 9.000000000000005329, 36.39999999999999147, 2.499999999999997335 ) ) ;
#12296 = CARTESIAN_POINT ( 'NONE',  ( 1.999999999999994449, -24.21594847648362858, -4.263001620021102944 ) ) ;
#12297 = CARTESIAN_POINT ( 'NONE',  ( -1.593127413382998459, 18.37180007765648071, -2.091722143975139669 ) ) ;
#12298 = VERTEX_POINT ( 'NONE', #6237 ) ;
#12299 = ORIENTED_EDGE ( 'NONE', *, *, #7385, .F. ) ;
#12300 = CARTESIAN_POINT ( 'NONE',  ( 0.000000000000000000, 34.19999999999999574, 2.500000000000000000 ) ) ;
#12301 = CARTESIAN_POINT ( 'NONE',  ( -4.499999999999999112, 37.00319992234354771, -0.05647727720528529505 ) ) ;
#12302 = CARTESIAN_POINT ( 'NONE',  ( 1.999999999999994449, -26.47440569391090648, -7.488412793402255296 ) ) ;
#12303 = CARTESIAN_POINT ( 'NONE',  ( -0.7188294034286550893, 27.50319992234354771, -2.395093729190349130 ) ) ;
#12304 = AXIS2_PLACEMENT_3D ( 'NONE', #11060, #11145, #13940 ) ;
#12305 = ORIENTED_EDGE ( 'NONE', *, *, #8930, .T. ) ;
#12306 = CARTESIAN_POINT ( 'NONE',  ( 2.121784821874994176, -28.88952095871037429, -10.56979653803383989 ) ) ;
#12307 = CARTESIAN_POINT ( 'NONE',  ( 2.733110507866247652, 23.87180007765647716, -3.862833514489153686 ) ) ;
#12308 = AXIS2_PLACEMENT_3D ( 'NONE', #4666, #7253, #1445 ) ;
#12309 = CARTESIAN_POINT ( 'NONE',  ( -3.999999999999997335, -18.49715259029829539, -6.161509441896827255 ) ) ;
#12310 = VERTEX_POINT ( 'NONE', #10025 ) ;
#12311 = CARTESIAN_POINT ( 'NONE',  ( 8.000000000000000000, 6.500000000000000000, 0.000000000000000000 ) ) ;
#12312 = FILL_AREA_STYLE ('',( #12406 ) ) ;
#12313 = CARTESIAN_POINT ( 'NONE',  ( 9.000000000000005329, -10.00000000000000000, 15.14468620625654616 ) ) ;
#12314 = EDGE_CURVE ( 'NONE', #6787, #13443, #16315, .T. ) ;
#12315 = CARTESIAN_POINT ( 'NONE',  ( 4.243569643750003451, -18.35507293947206264, -6.203770876333551954 ) ) ;
#12316 = CARTESIAN_POINT ( 'NONE',  ( 2.121784821875004390, -20.20155892317395541, -10.97657120925539154 ) ) ;
#12317 = EDGE_CURVE ( 'NONE', #13188, #9609, #7044, .T. ) ;
#12318 = CARTESIAN_POINT ( 'NONE',  ( -8.000000000000001776, 18.79999999999999361, 2.499999999999995115 ) ) ;
#12319 = EDGE_CURVE ( 'NONE', #8355, #9202, #17203, .T. ) ;
#12320 = ORIENTED_EDGE ( 'NONE', *, *, #818, .T. ) ;
#12321 = CARTESIAN_POINT ( 'NONE',  ( 4.000000000000000888, -24.69072647674599352, -10.98053173535865135 ) ) ;
#12322 = LINE ( 'NONE', #15308, #5387 ) ;
#12323 = PRESENTATION_STYLE_ASSIGNMENT (( #1030 ) ) ;
#12324 = ADVANCED_FACE ( 'NONE', ( #4655 ), #3507, .T. ) ;
#12325 = PRESENTATION_STYLE_ASSIGNMENT (( #12417 ) ) ;
#12326 = ORIENTED_EDGE ( 'NONE', *, *, #15350, .F. ) ;
#12327 = CARTESIAN_POINT ( 'NONE',  ( -3.500000000000000444, 34.50319992234354771, -0.05647727720529563400 ) ) ;
#12328 = CARTESIAN_POINT ( 'NONE',  ( 3.481649420246395010, 23.37819992234354061, 1.193696214020467439 ) ) ;
#12329 = CARTESIAN_POINT ( 'NONE',  ( -3.999999999999997335, -25.01441484904194823, -15.46912454613729793 ) ) ;
#12330 = CARTESIAN_POINT ( 'NONE',  ( 1.593127413382998903, 27.12180007765647716, 2.091722143975139669 ) ) ;
#12331 = CARTESIAN_POINT ( 'NONE',  ( -4.481649420246396787, 24.62819992234354416, -1.518615910253363399 ) ) ;
#12332 = CARTESIAN_POINT ( 'NONE',  ( 4.000000000000000888, -24.62619912695155477, -10.88837712936937230 ) ) ;
#12333 = ORIENTED_EDGE ( 'NONE', *, *, #4444, .F. ) ;
#12334 = LINE ( 'NONE', #13064, #7568 ) ;
#12335 = AXIS2_PLACEMENT_3D ( 'NONE', #5415, #18232, #15605 ) ;
#12336 = CARTESIAN_POINT ( 'NONE',  ( -4.481649420246366589, 37.87180007765647360, 1.518615910253458878 ) ) ;
#12337 = CARTESIAN_POINT ( 'NONE',  ( -2.121784821874996396, -20.90060520497677743, -11.97491276323260756 ) ) ;
#12338 = CARTESIAN_POINT ( 'NONE',  ( 4.000000000000000000, 1.759474945355381514, -3.047500000000001652 ) ) ;
#12339 = CARTESIAN_POINT ( 'NONE',  ( 1.071796769724476128, -18.00569549856575335, -8.407105251345607044 ) ) ;
#12340 = DIRECTION ( 'NONE',  ( 1.000000000000000000, 0.000000000000000000, 0.000000000000000000 ) ) ;
#12341 = VERTEX_POINT ( 'NONE', #4754 ) ;
#12342 = ORIENTED_EDGE ( 'NONE', *, *, #4378, .F. ) ;
#12343 = LINE ( 'NONE', #8173, #12973 ) ;
#12344 = DIRECTION ( 'NONE',  ( 0.000000000000000000, 0.000000000000000000, -1.000000000000000000 ) ) ;
#12345 = CYLINDRICAL_SURFACE ( 'NONE', #13678, 4.000000000000000000 ) ;
#12346 = CARTESIAN_POINT ( 'NONE',  ( 1.071796769724494780, -27.43958915976224944, -7.932527314431709442 ) ) ;
#12347 = VERTEX_POINT ( 'NONE', #14398 ) ;
#12348 = CARTESIAN_POINT ( 'NONE',  ( -1.497042530366522461, 34.87819992234354771, -2.161531897785030409 ) ) ;
#12349 = AXIS2_PLACEMENT_3D ( 'NONE', #13876, #18074, #8211 ) ;
#12350 = CARTESIAN_POINT ( 'NONE',  ( 2.121784821874994176, -27.82481969873374794, -9.049245555822391651 ) ) ;
#12351 = CARTESIAN_POINT ( 'NONE',  ( 1.135272562821090458, 27.24680007765648071, 3.311245368580554072 ) ) ;
#12352 = CARTESIAN_POINT ( 'NONE',  ( -3.500000000000000444, 29.50319992234354416, -0.05647727720529563400 ) ) ;
#12353 = CARTESIAN_POINT ( 'NONE',  ( 9.000000000000001776, 40.79999999999999716, -2.500000000000002665 ) ) ;
#12354 = CARTESIAN_POINT ( 'NONE',  ( -2.121784821874996396, -21.44908767223746437, -12.75822690558396033 ) ) ;
#12355 = EDGE_CURVE ( 'NONE', #9649, #2406, #9419, .T. ) ;
#12356 = AXIS2_PLACEMENT_3D ( 'NONE', #15657, #266, #1852 ) ;
#12357 = AXIS2_PLACEMENT_3D ( 'NONE', #9222, #6353, #13480 ) ;
#12358 = CARTESIAN_POINT ( 'NONE',  ( 0.000000000000000000, 1.443375672974065216, 7.222237291452134449E-31 ) ) ;
#12359 = CARTESIAN_POINT ( 'NONE',  ( -3.673772985318219053, 20.74680007765647716, -2.599342558260952174 ) ) ;
#12360 = DIRECTION ( 'NONE',  ( -1.000000000000000000, 0.000000000000000000, -0.000000000000000000 ) ) ;
#12361 = DIRECTION ( 'NONE',  ( -1.000000000000000000, 0.000000000000000000, 0.000000000000000000 ) ) ;
#12362 = CARTESIAN_POINT ( 'NONE',  ( 2.121784821875004390, -19.65307645591326846, -10.19325706690404054 ) ) ;
#12363 = CARTESIAN_POINT ( 'NONE',  ( 1.999999999999994449, -27.57137062913722048, -9.055041079111724400 ) ) ;
#12364 = CARTESIAN_POINT ( 'NONE',  ( 4.000000000000000888, -25.20694526946192937, -11.71776857521874504 ) ) ;
#12365 = CARTESIAN_POINT ( 'NONE',  ( 0.8262555684461332373, 34.74680007765647360, 2.360188852285403982 ) ) ;
#12366 = CARTESIAN_POINT ( 'NONE',  ( 3.999999999999996447, -22.40970851469716152, -3.696582572437044245 ) ) ;
#12367 = CARTESIAN_POINT ( 'NONE',  ( 2.864755990943265829, 39.49680007765647360, 2.011557305968487697 ) ) ;
#12368 = AXIS2_PLACEMENT_3D ( 'NONE', #15268, #15080, #5423 ) ;
#12369 = ITEM_DEFINED_TRANSFORMATION ( 'NONE', 'NONE', #16075,  #16940 ) ;
#12370 = VECTOR ( 'NONE', #10868, 1000.000000000000000 ) ;
#12371 = CARTESIAN_POINT ( 'NONE',  ( 9.000000000000001776, 18.79999999999999361, -2.500000000000002665 ) ) ;
#12372 = CIRCLE ( 'NONE', #9709, 2.149999999999995470 ) ;
#12373 = ADVANCED_FACE ( 'NONE', ( #497 ), #14693, .F. ) ;
#12374 = VERTEX_POINT ( 'NONE', #2267 ) ;
#12375 = CARTESIAN_POINT ( 'NONE',  ( -2.121784821875005722, -24.54467945335122536, -4.364719802544705374 ) ) ;
#12376 = UNCERTAINTY_MEASURE_WITH_UNIT (LENGTH_MEASURE( 1.000000000000000082E-05 ), #14154, 'distance_accuracy_value', 'NONE');
#12377 = CARTESIAN_POINT ( 'NONE',  ( -3.500000000000000444, 25.49680007765647716, 0.05647727720536892260 ) ) ;
#12378 = EDGE_CURVE ( 'NONE', #13359, #12413, #565, .T. ) ;
#12379 = ADVANCED_FACE ( 'NONE', ( #13739 ), #2920, .T. ) ;
#12380 = DIRECTION ( 'NONE',  ( -0.000000000000000000, -1.000000000000000000, -0.000000000000000000 ) ) ;
#12381 = CARTESIAN_POINT ( 'NONE',  ( -4.243569643750004339, -28.95075028426963826, -12.79298613310618471 ) ) ;
#12382 = AXIS2_PLACEMENT_3D ( 'NONE', #6894, #14039, #9402 ) ;
#12383 = CARTESIAN_POINT ( 'NONE',  ( -8.000000000000001776, 16.59999999999999787, 2.499999999999995115 ) ) ;
#12384=STYLED_ITEM('',(#18410),#14305);
#12385 = CARTESIAN_POINT ( 'NONE',  ( 2.000000000000004441, -23.55232074906610507, -15.39419672512663340 ) ) ;
#12387 = CARTESIAN_POINT ( 'NONE',  ( -4.000000000000004441, -23.59270991537611550, -5.386083664789866887 ) ) ;
#12386 = AXIS2_PLACEMENT_3D ( 'NONE', #2063, #17742, #3534 ) ;
#12388 = CARTESIAN_POINT ( 'NONE',  ( 4.730628863548789710E-15, -21.46729876507041013, -14.91998009733462816 ) ) ;
#12389 = ORIENTED_EDGE ( 'NONE', *, *, #13450, .F. ) ;
#12390 = DIRECTION ( 'NONE',  ( -0.000000000000000000, 1.000000000000000000, -0.000000000000000000 ) ) ;
#12391 = CARTESIAN_POINT ( 'NONE',  ( -4.000000000000004441, -23.07649112266017610, -4.648846824929771415 ) ) ;
#12392 = CARTESIAN_POINT ( 'NONE',  ( 2.798362969681366330, 36.49680007765648071, -2.102939460078824929 ) ) ;
#12393 = ORIENTED_EDGE ( 'NONE', *, *, #3325, .T. ) ;
#12394 =( BOUNDED_SURFACE ( )  B_SPLINE_SURFACE ( 1, 2, ( 
 ( #9089, #9275, #670, #12234, #10665, #14769, #5009, #14864, #10571, #11966, #6583, #3711, #16335, #7876, #14956, #7697, #13358, #6495, #10844, #6316, #12051, #9361, #17658, #4920, #16245, #2160, #13533, #12140, #10756, #17833, #7791, #5097, #17920, #16432, #13447, #761, #16520, #2341, #6406, #7974, #5192, #3798, #4885, #13225, #446, #11648, #12946, #16124, #7569, #10536, #16210, #3230, #1842, #540, #8867, #5993, #14446, #6186, #14543, #6087, #11737, #1752, #11835, #3131, #17244, #13325, #8964, #9057, #4517, #3502, #7476, #13136, #10161, #257, #7286, #13040, #14642, #11551, #4602, #17532, #4796, #5903, #15931, #17432, #17342, #3414, #14350, #4699, #10350, #8768, #10446, #11930, #14734, #7380, #1650, #16030, #10253, #17625, #15837, #2033, #3320, #1943, #7656, #637, #355, #6277, #10695, #16424, #17740, #845, #14950, #2333, #5091, #7784, #5002, #2152, #6214, #16514, #10659, #933, #11862, #11959, #2244, #13714, #17914, #17557, #10837, #17652, #10564, #13441, #663, #3705, #16152, #9267, #754, #4828, #9354, #13527, #6309, #9447, #16330, #7869, #7964, #15122, #10750, #3618, #3531, #10474, #13620, #17827, #2423, #8053, #6399, #12046, #15030, #6485, #16239, #4913, #6576, #12134, #3792, #12227, #3442, #5183, #14857, #2060, #9083, #14762, #7692, #13352, #9178, #15397, #11019, #16793, #17575, #8413, #7014, #5372, #1387, #13899, #16883, #11104, #12316, #12410, #5640, #13806, #9537, #16702, #1116, #12588, #8239, #11281, #14073, #16974, #18192, #9626, #15215, #5459, #1301, #10931, #12499, #5277, #2696, #3975, #4063, #4250, #12681, #9894, #15302, #15564, #1210, #4159, #9713, #18007, #18103, #2862, #6753, #2516, #2602, #8327, #6846, #13988, #8497, #1026, #8144, #6932, #18274, #5548, #11196, #6666, #9806, #16614, #15487, #2784, #3888, #13140, #1847, #7202, #8871, #15841, #14454, #4606, #14548, #10354, #11371, #261, #10257, #1476, #14169, #15937, #450, #78, #12859, #1654, #3135, #5908, #10165, #1756, #6091, #7112, #12773, #7291, #5731, #7482, #12952, #16033, #5999, #11556, #8772, #4523, #3234, #13046, #15747, #17248, #10069, #17061, #11740, #7384, #17438, #4333, #1566, #359, #3324, #4704, #9980, #15655, #166, #5817, #3049, #8590, #11653, #2955, #17346, #8677, #14263, #11460, #17152, #4427, #14354, #7759, #12021, #5069, #17890, #7849, #13420, #6282, #7573, #10724, #2223, #5162, #10816, #16214, #14832, #13502, #3509, #11838, #13229, #1947, #7660, #9244, #6190, #17629, #817, #12112, #545, #10539, #733, #11936, #16401, #8972, #6376, #2130, #16130, #6463, #6554, #3686, #14738, #16491, #17714, #4890, #12203, #14646, #9332, #4981, #10634, #16308, #15009, #17536, #17807 ),
 ( #3594, #2305, #4800, #911, #14930, #7939, #642, #13596, #9155, #10451, #13329, #3420, #9061, #2037, #1005, #15466, #5525, #14052, #9511, #12656, #6823, #6644, #11262, #9784, #12470, #3863, #9608, #2672, #15280, #9421, #4137, #1092, #2760, #1363, #16676, #15190, #11084, #3955, #13963, #16769, #18255, #13877, #18167, #2580, #8390, #8212, #18075, #5618, #1187, #6994, #10910, #15097, #18347, #3769, #2399, #5345, #11170, #12293, #6731, #8032, #16584, #5437, #4039, #17983, #9689, #10998, #13689, #5253, #16861, #2493, #8123, #15373, #8307, #13781, #1276, #12388, #6911, #12567, #11533, #11628, #7087, #6066, #5794, #10047, #4586, #14525, #11436, #4311, #5885, #17128, #8751, #17225, #13023, #8655, #7269, #4406, #17322, #15724, #12840, #428, #3023, #1822, #5710, #4229, #7459, #10235, #13119, #144, #336, #12752, #14240, #16951, #11351, #14334, #237, #14144, #1632, #12925, #9872, #15546, #5976, #54, #8847, #4499, #10139, #17040, #15821, #9958, #1457, #15912, #3117, #3210, #15633, #2843, #14425, #1728, #2933, #8473, #8568, #1544, #7362, #7179, #2013, #4957, #14904, #16009, #13306, #10518, #14715, #13481, #11720, #9129, #4868, #522, #10610, #9311, #795, #17512, #13569, #14809, #7640, #14985, #17414, #12088, #3482, #2107, #7735, #6441, #10330, #16286, #11816, #13395, #7825, #6257, #5046, #6354, #707, #7550, #1925, #618, #16190, #17786, #4679, #3666, #11996, #10701, #3396, #16378, #11910, #17605, #10427, #17691, #9038, #3574, #8943, #2286, #7915, #888, #4774, #3301, #9223, #14622, #13205, #6166, #2198, #16105, #12362, #5418, #18055, #12181, #6891, #3844, #15074, #12272, #13663, #6710, #2471, #18235, #1072, #15444, #16750, #5329, #9489, #5504, #12548, #17959, #1258, #8193, #6804, #15352, #11151, #2740, #3747, #10980, #2650, #17870, #6531, #8288, #16842, #10795, #5230, #16658, #13855, #3934, #2560, #12453, #4117, #5138, #16464, #9584, #9397, #9766, #15263, #8374, #4023, #1163, #18149, #11067, #13945, #9671, #8099, #14035, #13761, #2379, #8009, #983, #6627, #10885, #16564, #15165, #8827, #13001, #1343, #5953, #12734, #5687, #2912, #14124, #17204, #11245, #4381, #8545, #6974, #4475, #8634, #1437, #4569, #122, #10026, #15800, #10211, #215, #5774, #17023, #18326, #3094, #12904, #15891, #3188, #14220, #7158, #5864, #1524, #11330, #7065, #11511, #12820, #11608, #14400, #17303, #11415, #9940, #15529, #17107, #1612, #16932, #15703, #5598, #3001, #4293, #14313, #313, #8727, #7341, #15609, #1707, #7245, #10118, #12637, #4207, #35, #9854, #2826, #8453, #500, #10500, #1903, #6144, #14882, #17768, #17392, #13097, #7436, #13186, #14790, #11699, #4757, #7717, #17674 ) ),
 .UNSPECIFIED., .F., .F., .T. ) 
 B_SPLINE_SURFACE_WITH_KNOTS ( ( 2, 2 ),
 ( 3, 2, 2, 2, 2, 2, 2, 2, 2, 2, 2, 2, 2, 2, 2, 2, 2, 2, 2, 2, 2, 2, 2, 2, 2, 2, 2, 2, 2, 2, 2, 2, 2, 2, 2, 2, 2, 2, 2, 2, 2, 2, 2, 2, 2, 2, 2, 2, 2, 2, 2, 2, 2, 2, 2, 2, 2, 2, 2, 2, 2, 2, 2, 2, 2, 2, 2, 2, 2, 2, 2, 2, 2, 2, 2, 2, 2, 2, 2, 2, 2, 2, 2, 2, 2, 2, 2, 2, 2, 2, 2, 2, 2, 2, 2, 2, 2, 2, 2, 2, 2, 2, 2, 2, 2, 2, 2, 2, 2, 2, 2, 2, 2, 2, 2, 2, 2, 2, 2, 2, 2, 2, 2, 2, 2, 2, 2, 2, 2, 2, 2, 2, 2, 2, 2, 2, 2, 2, 2, 2, 2, 2, 2, 2, 2, 2, 2, 2, 2, 2, 2, 2, 2, 2, 2, 2, 2, 2, 2, 2, 2, 2, 2, 2, 2, 2, 2, 2, 2, 2, 2, 2, 2, 2, 3 ),
 ( 0.000000000000000000, 1.000000000000000000 ),
 ( 0.000000000000000000, 0.005747126436781609116, 0.01149425287356321823, 0.01724137931034482735, 0.02298850574712643646, 0.02873563218390804558, 0.03448275862068965469, 0.04022988505747126381, 0.04597701149425287293, 0.05172413793103448204, 0.05747126436781609116, 0.06321839080459770721, 0.06896551724137930939, 0.07471264367816092544, 0.08045977011494252762, 0.08620689655172414367, 0.09195402298850574585, 0.09770114942528736190, 0.1034482758620689641, 0.1091954022988505801, 0.1149425287356321823, 0.1206896551724137984, 0.1264367816091954144, 0.1321839080459770166, 0.1379310344827586188, 0.1436781609195402210, 0.1494252873563218509, 0.1551724137931034531, 0.1609195402298850552, 0.1666666666666666574, 0.1724137931034482873, 0.1781609195402298895, 0.1839080459770114917, 0.1896551724137930939, 0.1954022988505747238, 0.2011494252873563260, 0.2068965517241379282, 0.2126436781609195303, 0.2183908045977011603, 0.2241379310344827624, 0.2298850574712643646, 0.2356321839080459668, 0.2413793103448275967, 0.2471264367816091989, 0.2528735632183908288, 0.2586206896551724310, 0.2643678160919540332, 0.2701149425287356354, 0.2758620689655172376, 0.2816091954022988397, 0.2873563218390804419, 0.2931034482758620441, 0.2988505747126437018, 0.3045977011494253039, 0.3103448275862069061, 0.3160919540229885083, 0.3218390804597701105, 0.3275862068965517127, 0.3333333333333333148, 0.3390804597701149170, 0.3448275862068965747, 0.3505747126436781769, 0.3563218390804597790, 0.3620689655172413812, 0.3678160919540229834, 0.3735632183908045856, 0.3793103448275861878, 0.3850574712643677899, 0.3908045977011494476, 0.3965517241379310498, 0.4022988505747126520, 0.4080459770114942541, 0.4137931034482758563, 0.4195402298850574585, 0.4252873563218390607, 0.4310344827586206629, 0.4367816091954023205, 0.4425287356321839227, 0.4482758620689655249, 0.4540229885057471271, 0.4597701149425287293, 0.4655172413793103314, 0.4712643678160919336, 0.4770114942528735358, 0.4827586206896551935, 0.4885057471264367956, 0.4942528735632183978, 0.5000000000000000000, 0.5057471264367816577, 0.5114942528735632044, 0.5172413793103448620, 0.5229885057471264087, 0.5287356321839080664, 0.5344827586206896131, 0.5402298850574712707, 0.5459770114942529284, 0.5517241379310344751, 0.5574712643678161328, 0.5632183908045976795, 0.5689655172413793371, 0.5747126436781608838, 0.5804597701149425415, 0.5862068965517240882, 0.5919540229885057459, 0.5977011494252874035, 0.6034482758620689502, 0.6091954022988506079, 0.6149425287356321546, 0.6206896551724138122, 0.6264367816091953589, 0.6321839080459770166, 0.6379310344827586743, 0.6436781609195402210, 0.6494252873563218786, 0.6551724137931034253, 0.6609195402298850830, 0.6666666666666666297, 0.6724137931034482873, 0.6781609195402298340, 0.6839080459770114917, 0.6896551724137931494, 0.6954022988505746961, 0.7011494252873563537, 0.7068965517241379004, 0.7126436781609195581, 0.7183908045977011048, 0.7241379310344827624, 0.7298850574712644201, 0.7356321839080459668, 0.7413793103448276245, 0.7471264367816091712, 0.7528735632183908288, 0.7586206896551723755, 0.7643678160919540332, 0.7701149425287355799, 0.7758620689655172376, 0.7816091954022988952, 0.7873563218390804419, 0.7931034482758620996, 0.7988505747126436463, 0.8045977011494253039, 0.8103448275862068506, 0.8160919540229885083, 0.8218390804597701660, 0.8275862068965517127, 0.8333333333333333703, 0.8390804597701149170, 0.8448275862068965747, 0.8505747126436781214, 0.8563218390804597790, 0.8620689655172413257, 0.8678160919540229834, 0.8735632183908046411, 0.8793103448275861878, 0.8850574712643678454, 0.8908045977011493921, 0.8965517241379310498, 0.9022988505747125965, 0.9080459770114942541, 0.9137931034482759118, 0.9195402298850574585, 0.9252873563218391162, 0.9310344827586206629, 0.9367816091954023205, 0.9425287356321838672, 0.9482758620689655249, 0.9540229885057470716, 0.9597701149425287293, 0.9655172413793103869, 0.9712643678160919336, 0.9770114942528735913, 0.9827586206896551380, 0.9885057471264367956, 0.9942528735632183423, 0.9961881835133211682 ),
 .UNSPECIFIED. ) 
 GEOMETRIC_REPRESENTATION_ITEM ( )  RATIONAL_B_SPLINE_SURFACE ( (
 ( 1.000000000000000000, 0.8660254037844387076, 1.000000000000000000, 0.8660254037844387076, 1.000000000000000000, 0.8660254037844387076, 1.000000000000000000, 0.8660254037844387076, 1.000000000000000000, 0.8660254037844387076, 1.000000000000000000, 0.8660254037844387076, 1.000000000000000000, 0.8660254037844387076, 1.000000000000000000, 0.8660254037844387076, 1.000000000000000000, 0.8660254037844387076, 1.000000000000000000, 0.8660254037844387076, 1.000000000000000000, 0.8660254037844387076, 1.000000000000000000, 0.8660254037844387076, 1.000000000000000000, 0.8660254037844387076, 1.000000000000000000, 0.8660254037844387076, 1.000000000000000000, 0.8660254037844387076, 1.000000000000000000, 0.8660254037844387076, 1.000000000000000000, 0.8660254037844387076, 1.000000000000000000, 0.8660254037844387076, 1.000000000000000000, 0.8660254037844387076, 1.000000000000000000, 0.8660254037844387076, 1.000000000000000000, 0.8660254037844387076, 1.000000000000000000, 0.8660254037844387076, 1.000000000000000000, 0.8660254037844387076, 1.000000000000000000, 0.8660254037844387076, 1.000000000000000000, 0.8660254037844387076, 1.000000000000000000, 0.8660254037844387076, 1.000000000000000000, 0.8660254037844387076, 1.000000000000000000, 0.8660254037844387076, 1.000000000000000000, 0.8660254037844387076, 1.000000000000000000, 0.8660254037844387076, 1.000000000000000000, 0.8660254037844387076, 1.000000000000000000, 0.8660254037844387076, 1.000000000000000000, 0.8660254037844387076, 1.000000000000000000, 0.8660254037844387076, 1.000000000000000000, 0.8660254037844387076, 1.000000000000000000, 0.8660254037844387076, 1.000000000000000000, 0.8660254037844387076, 1.000000000000000000, 0.8660254037844387076, 1.000000000000000000, 0.8660254037844387076, 1.000000000000000000, 0.8660254037844387076, 1.000000000000000000, 0.8660254037844387076, 1.000000000000000000, 0.8660254037844387076, 1.000000000000000000, 0.8660254037844387076, 1.000000000000000000, 0.8660254037844387076, 1.000000000000000000, 0.8660254037844387076, 1.000000000000000000, 0.8660254037844387076, 1.000000000000000000, 0.8660254037844387076, 1.000000000000000000, 0.8660254037844387076, 1.000000000000000000, 0.8660254037844387076, 1.000000000000000000, 0.8660254037844387076, 1.000000000000000000, 0.8660254037844387076, 1.000000000000000000, 0.8660254037844387076, 1.000000000000000000, 0.8660254037844387076, 1.000000000000000000, 0.8660254037844387076, 1.000000000000000000, 0.8660254037844387076, 1.000000000000000000, 0.8660254037844387076, 1.000000000000000000, 0.8660254037844387076, 1.000000000000000000, 0.8660254037844387076, 1.000000000000000000, 0.8660254037844387076, 1.000000000000000000, 0.8660254037844387076, 1.000000000000000000, 0.8660254037844387076, 1.000000000000000000, 0.8660254037844387076, 1.000000000000000000, 0.8660254037844387076, 1.000000000000000000, 0.8660254037844387076, 1.000000000000000000, 0.8660254037844387076, 1.000000000000000000, 0.8660254037844387076, 1.000000000000000000, 0.8660254037844387076, 1.000000000000000000, 0.8660254037844387076, 1.000000000000000000, 0.8660254037844387076, 1.000000000000000000, 0.8660254037844387076, 1.000000000000000000, 0.8660254037844387076, 1.000000000000000000, 0.8660254037844387076, 1.000000000000000000, 0.8660254037844387076, 1.000000000000000000, 0.8660254037844387076, 1.000000000000000000, 0.8660254037844387076, 1.000000000000000000, 0.8660254037844387076, 1.000000000000000000, 0.8660254037844387076, 1.000000000000000000, 0.8660254037844387076, 1.000000000000000000, 0.8660254037844387076, 1.000000000000000000, 0.8660254037844387076, 1.000000000000000000, 0.8660254037844387076, 1.000000000000000000, 0.8660254037844387076, 1.000000000000000000, 0.8660254037844387076, 1.000000000000000000, 0.8660254037844387076, 1.000000000000000000, 0.8660254037844387076, 1.000000000000000000, 0.8660254037844387076, 1.000000000000000000, 0.8660254037844387076, 1.000000000000000000, 0.8660254037844387076, 1.000000000000000000, 0.8660254037844387076, 1.000000000000000000, 0.8660254037844387076, 1.000000000000000000, 0.8660254037844387076, 1.000000000000000000, 0.8660254037844387076, 1.000000000000000000, 0.8660254037844387076, 1.000000000000000000, 0.8660254037844387076, 1.000000000000000000, 0.8660254037844387076, 1.000000000000000000, 0.8660254037844387076, 1.000000000000000000, 0.8660254037844387076, 1.000000000000000000, 0.8660254037844387076, 1.000000000000000000, 0.8660254037844387076, 1.000000000000000000, 0.8660254037844387076, 1.000000000000000000, 0.8660254037844387076, 1.000000000000000000, 0.8660254037844387076, 1.000000000000000000, 0.8660254037844387076, 1.000000000000000000, 0.8660254037844387076, 1.000000000000000000, 0.8660254037844387076, 1.000000000000000000, 0.8660254037844387076, 1.000000000000000000, 0.8660254037844387076, 1.000000000000000000, 0.8660254037844387076, 1.000000000000000000, 0.8660254037844387076, 1.000000000000000000, 0.8660254037844387076, 1.000000000000000000, 0.8660254037844387076, 1.000000000000000000, 0.8660254037844387076, 1.000000000000000000, 0.8660254037844387076, 1.000000000000000000, 0.8660254037844387076, 1.000000000000000000, 0.8660254037844387076, 1.000000000000000000, 0.8660254037844387076, 1.000000000000000000, 0.8660254037844387076, 1.000000000000000000, 0.8660254037844387076, 1.000000000000000000, 0.8660254037844387076, 1.000000000000000000, 0.8660254037844387076, 1.000000000000000000, 0.8660254037844387076, 1.000000000000000000, 0.8660254037844387076, 1.000000000000000000, 0.8660254037844387076, 1.000000000000000000, 0.8660254037844387076, 1.000000000000000000, 0.8660254037844387076, 1.000000000000000000, 0.8660254037844387076, 1.000000000000000000, 0.8660254037844387076, 1.000000000000000000, 0.8660254037844387076, 1.000000000000000000, 0.8660254037844387076, 1.000000000000000000, 0.8660254037844387076, 1.000000000000000000, 0.8660254037844387076, 1.000000000000000000, 0.8660254037844387076, 1.000000000000000000, 0.8660254037844387076, 1.000000000000000000, 0.8660254037844387076, 1.000000000000000000, 0.8660254037844387076, 1.000000000000000000, 0.8660254037844387076, 1.000000000000000000, 0.8660254037844387076, 1.000000000000000000, 0.8660254037844387076, 1.000000000000000000, 0.8660254037844387076, 1.000000000000000000, 0.8660254037844387076, 1.000000000000000000, 0.8660254037844387076, 1.000000000000000000, 0.8660254037844387076, 1.000000000000000000, 0.8660254037844387076, 1.000000000000000000, 0.8660254037844387076, 1.000000000000000000, 0.8660254037844387076, 1.000000000000000000, 0.8660254037844387076, 1.000000000000000000, 0.8660254037844387076, 1.000000000000000000, 0.8660254037844387076, 1.000000000000000000, 0.8660254037844387076, 1.000000000000000000, 0.8660254037844387076, 1.000000000000000000, 0.8660254037844387076, 1.000000000000000000, 0.8660254037844387076, 1.000000000000000000, 0.8660254037844387076, 1.000000000000000000, 0.8660254037844387076, 1.000000000000000000, 0.8660254037844387076, 1.000000000000000000, 0.8660254037844387076, 1.000000000000000000, 0.8660254037844387076, 1.000000000000000000, 0.8660254037844387076, 1.000000000000000000, 0.8660254037844387076, 1.000000000000000000, 0.8660254037844387076, 1.000000000000000000, 0.8660254037844387076, 1.000000000000000000, 0.8660254037844387076, 1.000000000000000000, 0.8660254037844387076, 1.000000000000000000, 0.8660254037844387076, 1.000000000000000000, 0.8660254037844387076, 1.000000000000000000, 0.8660254037844387076, 1.000000000000000000, 0.8660254037844387076, 1.000000000000000000, 0.8660254037844387076, 1.000000000000000000, 0.8660254037844387076, 1.000000000000000000, 0.8660254037844387076, 1.000000000000000000, 0.8660254037844387076, 1.000000000000000000, 0.8660254037844387076, 1.000000000000000000, 0.8660254037844387076, 1.000000000000000000, 0.9548848677736452295, 0.9401542295229485813),
 ( 1.000000000000000000, 0.8660254037844387076, 1.000000000000000000, 0.8660254037844387076, 1.000000000000000000, 0.8660254037844387076, 1.000000000000000000, 0.8660254037844387076, 1.000000000000000000, 0.8660254037844387076, 1.000000000000000000, 0.8660254037844387076, 1.000000000000000000, 0.8660254037844387076, 1.000000000000000000, 0.8660254037844387076, 1.000000000000000000, 0.8660254037844387076, 1.000000000000000000, 0.8660254037844387076, 1.000000000000000000, 0.8660254037844387076, 1.000000000000000000, 0.8660254037844387076, 1.000000000000000000, 0.8660254037844387076, 1.000000000000000000, 0.8660254037844387076, 1.000000000000000000, 0.8660254037844387076, 1.000000000000000000, 0.8660254037844387076, 1.000000000000000000, 0.8660254037844387076, 1.000000000000000000, 0.8660254037844387076, 1.000000000000000000, 0.8660254037844387076, 1.000000000000000000, 0.8660254037844387076, 1.000000000000000000, 0.8660254037844387076, 1.000000000000000000, 0.8660254037844387076, 1.000000000000000000, 0.8660254037844387076, 1.000000000000000000, 0.8660254037844387076, 1.000000000000000000, 0.8660254037844387076, 1.000000000000000000, 0.8660254037844387076, 1.000000000000000000, 0.8660254037844387076, 1.000000000000000000, 0.8660254037844387076, 1.000000000000000000, 0.8660254037844387076, 1.000000000000000000, 0.8660254037844387076, 1.000000000000000000, 0.8660254037844387076, 1.000000000000000000, 0.8660254037844387076, 1.000000000000000000, 0.8660254037844387076, 1.000000000000000000, 0.8660254037844387076, 1.000000000000000000, 0.8660254037844387076, 1.000000000000000000, 0.8660254037844387076, 1.000000000000000000, 0.8660254037844387076, 1.000000000000000000, 0.8660254037844387076, 1.000000000000000000, 0.8660254037844387076, 1.000000000000000000, 0.8660254037844387076, 1.000000000000000000, 0.8660254037844387076, 1.000000000000000000, 0.8660254037844387076, 1.000000000000000000, 0.8660254037844387076, 1.000000000000000000, 0.8660254037844387076, 1.000000000000000000, 0.8660254037844387076, 1.000000000000000000, 0.8660254037844387076, 1.000000000000000000, 0.8660254037844387076, 1.000000000000000000, 0.8660254037844387076, 1.000000000000000000, 0.8660254037844387076, 1.000000000000000000, 0.8660254037844387076, 1.000000000000000000, 0.8660254037844387076, 1.000000000000000000, 0.8660254037844387076, 1.000000000000000000, 0.8660254037844387076, 1.000000000000000000, 0.8660254037844387076, 1.000000000000000000, 0.8660254037844387076, 1.000000000000000000, 0.8660254037844387076, 1.000000000000000000, 0.8660254037844387076, 1.000000000000000000, 0.8660254037844387076, 1.000000000000000000, 0.8660254037844387076, 1.000000000000000000, 0.8660254037844387076, 1.000000000000000000, 0.8660254037844387076, 1.000000000000000000, 0.8660254037844387076, 1.000000000000000000, 0.8660254037844387076, 1.000000000000000000, 0.8660254037844387076, 1.000000000000000000, 0.8660254037844387076, 1.000000000000000000, 0.8660254037844387076, 1.000000000000000000, 0.8660254037844387076, 1.000000000000000000, 0.8660254037844387076, 1.000000000000000000, 0.8660254037844387076, 1.000000000000000000, 0.8660254037844387076, 1.000000000000000000, 0.8660254037844387076, 1.000000000000000000, 0.8660254037844387076, 1.000000000000000000, 0.8660254037844387076, 1.000000000000000000, 0.8660254037844387076, 1.000000000000000000, 0.8660254037844387076, 1.000000000000000000, 0.8660254037844387076, 1.000000000000000000, 0.8660254037844387076, 1.000000000000000000, 0.8660254037844387076, 1.000000000000000000, 0.8660254037844387076, 1.000000000000000000, 0.8660254037844387076, 1.000000000000000000, 0.8660254037844387076, 1.000000000000000000, 0.8660254037844387076, 1.000000000000000000, 0.8660254037844387076, 1.000000000000000000, 0.8660254037844387076, 1.000000000000000000, 0.8660254037844387076, 1.000000000000000000, 0.8660254037844387076, 1.000000000000000000, 0.8660254037844387076, 1.000000000000000000, 0.8660254037844387076, 1.000000000000000000, 0.8660254037844387076, 1.000000000000000000, 0.8660254037844387076, 1.000000000000000000, 0.8660254037844387076, 1.000000000000000000, 0.8660254037844387076, 1.000000000000000000, 0.8660254037844387076, 1.000000000000000000, 0.8660254037844387076, 1.000000000000000000, 0.8660254037844387076, 1.000000000000000000, 0.8660254037844387076, 1.000000000000000000, 0.8660254037844387076, 1.000000000000000000, 0.8660254037844387076, 1.000000000000000000, 0.8660254037844387076, 1.000000000000000000, 0.8660254037844387076, 1.000000000000000000, 0.8660254037844387076, 1.000000000000000000, 0.8660254037844387076, 1.000000000000000000, 0.8660254037844387076, 1.000000000000000000, 0.8660254037844387076, 1.000000000000000000, 0.8660254037844387076, 1.000000000000000000, 0.8660254037844387076, 1.000000000000000000, 0.8660254037844387076, 1.000000000000000000, 0.8660254037844387076, 1.000000000000000000, 0.8660254037844387076, 1.000000000000000000, 0.8660254037844387076, 1.000000000000000000, 0.8660254037844387076, 1.000000000000000000, 0.8660254037844387076, 1.000000000000000000, 0.8660254037844387076, 1.000000000000000000, 0.8660254037844387076, 1.000000000000000000, 0.8660254037844387076, 1.000000000000000000, 0.8660254037844387076, 1.000000000000000000, 0.8660254037844387076, 1.000000000000000000, 0.8660254037844387076, 1.000000000000000000, 0.8660254037844387076, 1.000000000000000000, 0.8660254037844387076, 1.000000000000000000, 0.8660254037844387076, 1.000000000000000000, 0.8660254037844387076, 1.000000000000000000, 0.8660254037844387076, 1.000000000000000000, 0.8660254037844387076, 1.000000000000000000, 0.8660254037844387076, 1.000000000000000000, 0.8660254037844387076, 1.000000000000000000, 0.8660254037844387076, 1.000000000000000000, 0.8660254037844387076, 1.000000000000000000, 0.8660254037844387076, 1.000000000000000000, 0.8660254037844387076, 1.000000000000000000, 0.8660254037844387076, 1.000000000000000000, 0.8660254037844387076, 1.000000000000000000, 0.8660254037844387076, 1.000000000000000000, 0.8660254037844387076, 1.000000000000000000, 0.8660254037844387076, 1.000000000000000000, 0.8660254037844387076, 1.000000000000000000, 0.8660254037844387076, 1.000000000000000000, 0.8660254037844387076, 1.000000000000000000, 0.8660254037844387076, 1.000000000000000000, 0.8660254037844387076, 1.000000000000000000, 0.8660254037844387076, 1.000000000000000000, 0.8660254037844387076, 1.000000000000000000, 0.8660254037844387076, 1.000000000000000000, 0.8660254037844387076, 1.000000000000000000, 0.8660254037844387076, 1.000000000000000000, 0.8660254037844387076, 1.000000000000000000, 0.8660254037844387076, 1.000000000000000000, 0.8660254037844387076, 1.000000000000000000, 0.8660254037844387076, 1.000000000000000000, 0.8660254037844387076, 1.000000000000000000, 0.8660254037844387076, 1.000000000000000000, 0.8660254037844387076, 1.000000000000000000, 0.8660254037844387076, 1.000000000000000000, 0.8660254037844387076, 1.000000000000000000, 0.8660254037844387076, 1.000000000000000000, 0.8660254037844387076, 1.000000000000000000, 0.8660254037844387076, 1.000000000000000000, 0.8660254037844387076, 1.000000000000000000, 0.8660254037844387076, 1.000000000000000000, 0.8660254037844387076, 1.000000000000000000, 0.8660254037844387076, 1.000000000000000000, 0.8660254037844387076, 1.000000000000000000, 0.8660254037844387076, 1.000000000000000000, 0.8660254037844387076, 1.000000000000000000, 0.8660254037844387076, 1.000000000000000000, 0.8660254037844387076, 1.000000000000000000, 0.8660254037844387076, 1.000000000000000000, 0.8660254037844387076, 1.000000000000000000, 0.8660254037844387076, 1.000000000000000000, 0.8660254037844387076, 1.000000000000000000, 0.8660254037844387076, 1.000000000000000000, 0.8660254037844387076, 1.000000000000000000, 0.8660254037844387076, 1.000000000000000000, 0.9548848677736452295, 0.9401542295229485813) ) ) 
 REPRESENTATION_ITEM ( '' )  SURFACE ( )  );
#12395 = CARTESIAN_POINT ( 'NONE',  ( 4.000000000000000888, -22.36774190952427688, -7.662965955988220834 ) ) ;
#12396 = CARTESIAN_POINT ( 'NONE',  ( 3.607379964056363075, 33.50319992234354061, 2.690724712371229010 ) ) ;
#12397 = CARTESIAN_POINT ( 'NONE',  ( -31.74999999999995737, 0.000000000000000000, 4.000000000000001776 ) ) ;
#12398 = CARTESIAN_POINT ( 'NONE',  ( -2.055738996568281518, 29.25319992234355126, 1.423772053676066962 ) ) ;
#12399 = VERTEX_POINT ( 'NONE', #16169 ) ;
#12400 = CARTESIAN_POINT ( 'NONE',  ( 4.243569643749997233, -27.09021171885596146, -10.13586168944375387 ) ) ;
#12401 = CIRCLE ( 'NONE', #4403, 0.9999999999999991118 ) ;
#12402 = CARTESIAN_POINT ( 'NONE',  ( -1.444289557196047014, 25.99680007765648071, -4.262301884875704161 ) ) ;
#12403 = CARTESIAN_POINT ( 'NONE',  ( 4.000000000000003553, -19.09940784846689610, -7.021619088400267827 ) ) ;
#12404 = ORIENTED_EDGE ( 'NONE', *, *, #379, .T. ) ;
#12405 = CARTESIAN_POINT ( 'NONE',  ( 1.300000000000000044, -1.443375672974064328, 2.168404344971008868E-16 ) ) ;
#12406 = FILL_AREA_STYLE_COLOUR ( '', #17451 ) ;
#12407 = DIRECTION ( 'NONE',  ( 0.000000000000000000, 1.000000000000000000, 0.000000000000000000 ) ) ;
#12408 = CIRCLE ( 'NONE', #10988, 2.000000000000001776 ) ;
#12409 = CARTESIAN_POINT ( 'NONE',  ( -8.500000000000005329, 10.00000000000000000, 20.49999999999999645 ) ) ;
#12410 = CARTESIAN_POINT ( 'NONE',  ( 4.730628863548789710E-15, -19.17657787239344458, -11.64849162045545583 ) ) ;
#12411 = VECTOR ( 'NONE', #9606, 1000.000000000000000 ) ;
#12412 = CARTESIAN_POINT ( 'NONE',  ( -3.113145992481321400, -29.13892139834124606, -12.87460258714478911 ) ) ;
#12413 = VERTEX_POINT ( 'NONE', #14970 ) ;
#12414 = CARTESIAN_POINT ( 'NONE',  ( 4.713407268011036227E-15, -21.35891669415256899, -14.27485004966103510 ) ) ;
#12415 = CARTESIAN_POINT ( 'NONE',  ( 1.071796769724485454, -21.81280909414084235, -13.84422694430704226 ) ) ;
#12416 = CARTESIAN_POINT ( 'NONE',  ( -2.798362969681365886, 17.74680007765647716, 2.102939460078824929 ) ) ;
#12417 = SURFACE_STYLE_USAGE ( .BOTH. , #849 ) ;
#12418 = VERTEX_POINT ( 'NONE', #8079 ) ;
#12419 = CARTESIAN_POINT ( 'NONE',  ( 3.518350579753605434, 35.62819992234353350, -1.080741659609877114 ) ) ;
#12420 = CARTESIAN_POINT ( 'NONE',  ( -1.135272562821019626, 16.50319992234354416, 3.311245368580577164 ) ) ;
#12421 = CARTESIAN_POINT ( 'NONE',  ( -4.243569643750000786, -19.99636183013295820, -4.276284222377527477 ) ) ;
#12422 = CARTESIAN_POINT ( 'NONE',  ( 0.05938372350926800214, 27.37180007765647716, 2.628655560595669183 ) ) ;
#12423 = CARTESIAN_POINT ( 'NONE',  ( -4.518350579753602325, 21.87819992234354416, 1.405661355842794391 ) ) ;
#12424 = CARTESIAN_POINT ( 'NONE',  ( 4.713407268011036227E-15, -20.52006115528422825, -13.07684018388161817 ) ) ;
#12425 = ORIENTED_EDGE ( 'NONE', *, *, #319, .F. ) ;
#12426 = EDGE_CURVE ( 'NONE', #8485, #8354, #5210, .T. ) ;
#12427 = CIRCLE ( 'NONE', #302, 3.047499999999999876 ) ;
#12428 = CARTESIAN_POINT ( 'NONE',  ( 4.243569643750000786, -20.41578959921466918, -4.875289154763852828 ) ) ;
#12429 = CARTESIAN_POINT ( 'NONE',  ( 3.500000000000000444, 19.24680007765648071, -0.05647727720536935281 ) ) ;
#12430 = ADVANCED_FACE ( 'NONE', ( #774 ), #7807, .F. ) ;
#12431 = CARTESIAN_POINT ( 'NONE',  ( 1.533898589781675205E-14, -27.51564321027552040, -8.041143755076902266 ) ) ;
#12432 = CARTESIAN_POINT ( 'NONE',  ( 4.243569643749997233, -26.79983864795324422, -9.721165967022450616 ) ) ;
#12433 = DIRECTION ( 'NONE',  ( 3.469446951953612217E-16, -0.000000000000000000, 1.000000000000000000 ) ) ;
#12434 = CARTESIAN_POINT ( 'NONE',  ( 4.000000000000000888, -21.33530432409240163, -6.188492276268029890 ) ) ;
#12435 = DIRECTION ( 'NONE',  ( 0.000000000000000000, 0.000000000000000000, -1.000000000000000000 ) ) ;
#12436 = EDGE_LOOP ( 'NONE', ( #13782, #17880, #5019, #10915, #9917, #2029 ) ) ;
#12437 = ORIENTED_EDGE ( 'NONE', *, *, #15775, .F. ) ;
#12438 = CARTESIAN_POINT ( 'NONE',  ( -2.864755990943265829, 18.24680007765648071, -2.011557305968488141 ) ) ;
#12439 = CARTESIAN_POINT ( 'NONE',  ( -1.071796769724486786, -18.69244293640756283, -9.387882235834636546 ) ) ;
#12440 = CYLINDRICAL_SURFACE ( 'NONE', #5676, 0.9999999999999991118 ) ;
#12441 = CARTESIAN_POINT ( 'NONE',  ( 1.300000000000000044, 0.7216878364870329410, 1.249999999999999778 ) ) ;
#12442 = VERTEX_POINT ( 'NONE', #3463 ) ;
#12443 = VECTOR ( 'NONE', #15887, 1000.000000000000000 ) ;
#12444 = CARTESIAN_POINT ( 'NONE',  ( 2.518350579753611207, 38.12819992234354771, -0.7558219633769606149 ) ) ;
#12445 = CARTESIAN_POINT ( 'NONE',  ( -4.243569643749997233, -21.88256802303096293, -11.24155594871087338 ) ) ;
#12446 = CARTESIAN_POINT ( 'NONE',  ( 2.798362969681366330, 33.99680007765648071, -2.102939460078824929 ) ) ;
#12447 = CARTESIAN_POINT ( 'NONE',  ( -2.798362969681409851, 24.75319992234354416, -2.102939460078765421 ) ) ;
#12448 = CARTESIAN_POINT ( 'NONE',  ( 8.000000000000000000, 34.19999999999999574, -2.500000000000000888 ) ) ;
#12449 = CARTESIAN_POINT ( 'NONE',  ( 4.730628863548789710E-15, -19.69279666510938043, -12.38572846031554953 ) ) ;
#12450 = EDGE_CURVE ( 'NONE', #13335, #10567, #5027, .T. ) ;
#12451 = CARTESIAN_POINT ( 'NONE',  ( 2.319183558094505493, -24.28745349265258469, -16.12279146867029667 ) ) ;
#12452 = CARTESIAN_POINT ( 'NONE',  ( 1.533898589781675205E-14, -27.25753381391755426, -7.672525335146852754 ) ) ;
#12453 = CARTESIAN_POINT ( 'NONE',  ( -4.243569643749997233, -19.81769285216720888, -8.292608589270493269 ) ) ;
#12454 = DIRECTION ( 'NONE',  ( -0.000000000000000000, 0.000000000000000000, -1.000000000000000000 ) ) ;
#12455 = CARTESIAN_POINT ( 'NONE',  ( 20.00000000000000355, 4.475777889183788807E-16, -3.309499999999999886 ) ) ;
#12456 = CARTESIAN_POINT ( 'NONE',  ( -1.497042530366477164, 35.12180007765647360, 2.161531897785062384 ) ) ;
#12457 = AXIS2_PLACEMENT_3D ( 'NONE', #18272, #6572, #1024 ) ;
#12458 = DIRECTION ( 'NONE',  ( -3.469446951953613696E-16, -0.000000000000000000, -1.000000000000000000 ) ) ;
#12459 = CARTESIAN_POINT ( 'NONE',  ( 2.211161402132902243, 37.12180007765647360, 2.942372952327172442 ) ) ;
#12460 = CARTESIAN_POINT ( 'NONE',  ( 1.300000000000000044, 0.000000000000000000, 0.000000000000000000 ) ) ;
#12461 = VECTOR ( 'NONE', #1606, 1000.000000000000000 ) ;
#12462 = CARTESIAN_POINT ( 'NONE',  ( -1.734723475976807094E-15, 43.00000000000000000, -2.500000000000000000 ) ) ;
#12463 = ADVANCED_BREP_SHAPE_REPRESENTATION ( '', ( #14467, #16940 ), #5661 ) ;
#12464 = EDGE_LOOP ( 'NONE', ( #2856, #7314, #9571, #104 ) ) ;
#12465 = CARTESIAN_POINT ( 'NONE',  ( 2.121784821874994176, -24.24355182426693389, -3.934664979292979314 ) ) ;
#12466 = CARTESIAN_POINT ( 'NONE',  ( 1.135272562821090458, 27.24680007765648071, 3.311245368580554072 ) ) ;
#12467 = CARTESIAN_POINT ( 'NONE',  ( 0.000000000000000000, 25.39999999999999503, 2.500000000000000000 ) ) ;
#12468 = DIRECTION ( 'NONE',  ( -0.000000000000000000, -0.5735764363510414965, -0.8191520442889950182 ) ) ;
#12469 = DIRECTION ( 'NONE',  ( -0.000000000000000000, -1.000000000000000000, -0.000000000000000000 ) ) ;
#12470 = CARTESIAN_POINT ( 'NONE',  ( 4.243569643750000786, -26.57815143726116602, -13.67605393059374208 ) ) ;
#12471 = ADVANCED_FACE ( 'NONE', ( #13372 ), #2908, .T. ) ;
#12472 = ORIENTED_EDGE ( 'NONE', *, *, #4423, .F. ) ;
#12473 = DIRECTION ( 'NONE',  ( 0.000000000000000000, 0.000000000000000000, 1.000000000000000000 ) ) ;
#12474 = CARTESIAN_POINT ( 'NONE',  ( -3.999999999999997335, -20.11033631824054524, -8.465374567466390943 ) ) ;
#12475 = CARTESIAN_POINT ( 'NONE',  ( 2.115076519116362963, 38.87180007765645939, -3.012182706137107147 ) ) ;
#12476 = EDGE_CURVE ( 'NONE', #17908, #12048, #1740, .T. ) ;
#12477 = ORIENTED_EDGE ( 'NONE', *, *, #2424, .T. ) ;
#12478 = CARTESIAN_POINT ( 'NONE',  ( 4.299564228933482956E-15, -22.89824732864832768, -15.39439339536058959 ) ) ;
#12479 = CIRCLE ( 'NONE', #5088, 10.00000000000000178 ) ;
#12480 = ADVANCED_FACE ( 'NONE', ( #9201 ), #16541, .F. ) ;
#12481 = CARTESIAN_POINT ( 'NONE',  ( 0.05938372350919016857, 35.12819992234354771, -4.731580009072201776 ) ) ;
#12482 = UNCERTAINTY_MEASURE_WITH_UNIT (LENGTH_MEASURE( 1.000000000000000082E-05 ), #443, 'distance_accuracy_value', 'NONE');
#12483 = VECTOR ( 'NONE', #6145, 1000.000000000000000 ) ;
#12484 = DIRECTION ( 'NONE',  ( 0.000000000000000000, 0.000000000000000000, -1.000000000000000000 ) ) ;
#12485 = CARTESIAN_POINT ( 'NONE',  ( 1.593127413382953383, 25.37819992234354416, -2.091722143975172532 ) ) ;
#12486 = EDGE_LOOP ( 'NONE', ( #8171, #2038, #11133, #6490 ) ) ;
#12487 = CARTESIAN_POINT ( 'NONE',  ( -2.121784821874996396, -22.48152525766933962, -14.23270058530414950 ) ) ;
#12488 = EDGE_CURVE ( 'NONE', #11229, #12007, #18033, .T. ) ;
#12489 = CARTESIAN_POINT ( 'NONE',  ( -1.336863392178478716, 24.99680007765647716, 4.297206761780677731 ) ) ;
#12490 = CARTESIAN_POINT ( 'NONE',  ( 4.000000000000003553, -18.84129845210892640, -6.653000668470220980 ) ) ;
#12491 = VERTEX_POINT ( 'NONE', #14787 ) ;
#12492 = DIRECTION ( 'NONE',  ( 1.000000000000000000, -0.000000000000000000, -0.000000000000000000 ) ) ;
#12493 = FACE_OUTER_BOUND ( 'NONE', #11000, .T. ) ;
#12494 = EDGE_CURVE ( 'NONE', #14506, #12849, #10589, .T. ) ;
#12495 = CARTESIAN_POINT ( 'NONE',  ( 19.30950000000002120, 0.000000000000000000, 0.000000000000000000 ) ) ;
#12496 = CARTESIAN_POINT ( 'NONE',  ( -8.500000000000005329, 13.00000000000000000, -22.64999999999999147 ) ) ;
#12497 = AXIS2_PLACEMENT_3D ( 'NONE', #2250, #3625, #7875 ) ;
#12498 =( BOUNDED_CURVE ( )  B_SPLINE_CURVE ( 2, ( #8166, #8676, #3909, #18028, #2446, #8077, #14168, #5907, #10068 ),
 .UNSPECIFIED., .F., .T. ) 
 B_SPLINE_CURVE_WITH_KNOTS ( ( 3, 2, 2, 2, 3 ),
 ( 0.8706896551724138122, 0.8735632183908046411, 0.8793103448275861878, 0.8850574712643678454, 0.8879310344827586743 ),
 .UNSPECIFIED. ) 
 CURVE ( )  GEOMETRIC_REPRESENTATION_ITEM ( )  RATIONAL_B_SPLINE_CURVE ( ( 0.9330127018922194093, 0.9330127018922194093, 1.000000000000000000, 0.8660254037844387076, 1.000000000000000000, 0.8660254037844387076, 1.000000000000000000, 0.9330127018922180770, 0.9330127018922194093 ) ) 
 REPRESENTATION_ITEM ( '' )  );
#12499 = CARTESIAN_POINT ( 'NONE',  ( -2.121784821875005722, -25.83522643514106676, -6.207811902194944054 ) ) ;
#12500 = ORIENTED_EDGE ( 'NONE', *, *, #15796, .T. ) ;
#12501 = CYLINDRICAL_SURFACE ( 'NONE', #18345, 0.9999999999999991118 ) ;
#12502 = VERTEX_POINT ( 'NONE', #17671 ) ;
#12503 = AXIS2_PLACEMENT_3D ( 'NONE', #6370, #11833, #1749 ) ;
#12504 = CARTESIAN_POINT ( 'NONE',  ( -2.000000000000005773, -27.87249825822150839, -9.485095902363450904 ) ) ;
#12505 = DIRECTION ( 'NONE',  ( -3.373073425510457965E-16, 0.000000000000000000, -1.000000000000000000 ) ) ;
#12506 = PLANE ( 'NONE',  #10143 ) ;
#12507 = FILL_AREA_STYLE_COLOUR ( '', #5403 ) ;
#12508 = ORIENTED_EDGE ( 'NONE', *, *, #9034, .T. ) ;
#12509 = CARTESIAN_POINT ( 'NONE',  ( 1.027846397803612311, 36.25319992234354771, 3.346150245485499219 ) ) ;
#12510 = CARTESIAN_POINT ( 'NONE',  ( 2.798362969681409851, 18.50319992234354771, 2.102939460078764977 ) ) ;
#12511 = CARTESIAN_POINT ( 'NONE',  ( -4.000000000000004441, -28.23867904981954879, -12.02121522353072969 ) ) ;
#12512 = CARTESIAN_POINT ( 'NONE',  ( -0.05938372350926768989, 26.12180007765648426, -2.628655560595669183 ) ) ;
#12513 = CIRCLE ( 'NONE', #12814, 0.9999999999999991118 ) ;
#12514 = CARTESIAN_POINT ( 'NONE',  ( -4.518350579753602325, 29.37819992234355126, 1.405661355842794391 ) ) ;
#12515 = VECTOR ( 'NONE', #12865, 1000.000000000000000 ) ;
#12516 = UNCERTAINTY_MEASURE_WITH_UNIT (LENGTH_MEASURE( 1.000000000000000082E-05 ), #1395, 'distance_accuracy_value', 'NONE');
#12517 = CARTESIAN_POINT ( 'NONE',  ( -2.000000000000005773, -27.03364271935316765, -8.287086036584028648 ) ) ;
#12518 = ORIENTED_EDGE ( 'NONE', *, *, #9880, .F. ) ;
#12519 = CARTESIAN_POINT ( 'NONE',  ( 3.999999999999996891, -2.343145750507611869, 16.84997118393183513 ) ) ;
#12520 = CARTESIAN_POINT ( 'NONE',  ( -2.115076519116362519, 20.12180007765648071, 3.012182706137107147 ) ) ;
#12521 = CARTESIAN_POINT ( 'NONE',  ( -4.000000000000004441, -26.17380387895579830, -9.072267864090346023 ) ) ;
#12522 = CARTESIAN_POINT ( 'NONE',  ( 4.243569643750003451, -20.41994811033580959, -9.152718235773933841 ) ) ;
#12523 = EDGE_CURVE ( 'NONE', #13188, #11611, #11191, .T. ) ;
#12524 = VECTOR ( 'NONE', #17795, 1000.000000000000000 ) ;
#12525 = AXIS2_PLACEMENT_3D ( 'NONE', #578, #478, #8899 ) ;
#12526 = CARTESIAN_POINT ( 'NONE',  ( -5.577813053751546416E-15, -24.35380310418546657, -3.525568109927051275 ) ) ;
#12527 = DIRECTION ( 'NONE',  ( 0.000000000000000000, 0.000000000000000000, -1.000000000000000000 ) ) ;
#12528 = ORIENTED_EDGE ( 'NONE', *, *, #7896, .F. ) ;
#12529 = ORIENTED_EDGE ( 'NONE', *, *, #4221, .F. ) ;
#12530 = CARTESIAN_POINT ( 'NONE',  ( -3.500000000000000444, 15.49680007765647893, 0.05647727720536892260 ) ) ;
#12531 = CARTESIAN_POINT ( 'NONE',  ( 0.000000000000000000, 3.000000000000000000, 0.000000000000000000 ) ) ;
#12532 = DIRECTION ( 'NONE',  ( 0.8191520442889951292, 0.4698463103929519935, -0.3289899283371605643 ) ) ;
#12533 = SURFACE_SIDE_STYLE ('',( #1421 ) ) ;
#12534 = ORIENTED_EDGE ( 'NONE', *, *, #6901, .F. ) ;
#12535 = CARTESIAN_POINT ( 'NONE',  ( 2.481649420246391902, 38.37819992234354061, 0.8687765177875720335 ) ) ;
#12536 = CARTESIAN_POINT ( 'NONE',  ( -4.243569643750005227, -26.36965632068995191, -9.106801933805707350 ) ) ;
#12537 = CARTESIAN_POINT ( 'NONE',  ( -2.115076519116362519, 35.12180007765645939, 3.012182706137107147 ) ) ;
#12538 = CARTESIAN_POINT ( 'NONE',  ( 0.05938372350920109732, 30.12819992234354416, -3.680117784833935701 ) ) ;
#12539 = DIRECTION ( 'NONE',  ( -0.000000000000000000, -1.000000000000000000, -0.000000000000000000 ) ) ;
#12540 = CARTESIAN_POINT ( 'NONE',  ( 1.300000000000000044, 0.7216878364870329410, -1.250000000000000000 ) ) ;
#12541 = VECTOR ( 'NONE', #419, 1000.000000000000000 ) ;
#12542 = CARTESIAN_POINT ( 'NONE',  ( 4.243569643750003451, -21.48464937031242883, -10.67326921798538386 ) ) ;
#12543 = DIRECTION ( 'NONE',  ( -1.000000000000000000, 0.000000000000000000, 4.336808689942021680E-16 ) ) ;
#12544 = ADVANCED_FACE ( 'NONE', ( #9377 ), #15053, .T. ) ;
#12545 = AXIS2_PLACEMENT_3D ( 'NONE', #16700, #7960, #10929 ) ;
#12546 = DIRECTION ( 'NONE',  ( 0.000000000000000000, -1.000000000000000000, 0.000000000000000000 ) ) ;
#12547 = FACE_OUTER_BOUND ( 'NONE', #17842, .T. ) ;
#12548 = CARTESIAN_POINT ( 'NONE',  ( -2.121784821875005722, -25.28674396788038337, -5.424497759843593059 ) ) ;
#12549 = CONICAL_SURFACE ( 'NONE', #9601, 1732.050807568857181, 1.047197551196592746 ) ;
#12550 = CARTESIAN_POINT ( 'NONE',  ( -1.071796769724496334, -25.20418534377263953, -4.740039810362389083 ) ) ;
#12551 = CARTESIAN_POINT ( 'NONE',  ( 8.500000000000019540, 0.000000000000000000, 20.49999999999998934 ) ) ;
#12552 = CARTESIAN_POINT ( 'NONE',  ( 2.518350579753611207, 15.62819992234354594, -0.7558219633769606149 ) ) ;
#12553 = ADVANCED_FACE ( 'NONE', ( #12251 ), #3817, .T. ) ;
#12554 = CARTESIAN_POINT ( 'NONE',  ( -3.706921591972381904E-14, -18.96207903348436119, -9.772962490420598058 ) ) ;
#12555 = FACE_BOUND ( 'NONE', #16850, .T. ) ;
#12556 = DIRECTION ( 'NONE',  ( 0.000000000000000000, -0.5735764363510414965, -0.8191520442889950182 ) ) ;
#12557 = CONTEXT_DEPENDENT_SHAPE_REPRESENTATION ( #17702, #16739 ) ;
#12558 = CARTESIAN_POINT ( 'NONE',  ( -8.500000000000005329, -1.201721234452885367, 20.49999999999999645 ) ) ;
#12559 = CIRCLE ( 'NONE', #13452, 0.9999999999999991118 ) ;
#12560 = ORIENTED_EDGE ( 'NONE', *, *, #11082, .T. ) ;
#12561 = CARTESIAN_POINT ( 'NONE',  ( 2.121784821875004390, -18.91101194138411046, -9.133479109605152857 ) ) ;
#12562 = CARTESIAN_POINT ( 'NONE',  ( -3.500000000000000444, 35.49680007765648071, 0.05647727720536892260 ) ) ;
#12563 = CARTESIAN_POINT ( 'NONE',  ( 9.000000000000000000, 36.39999999999999147, -2.500000000000001332 ) ) ;
#12564 = FACE_OUTER_BOUND ( 'NONE', #10989, .T. ) ;
#12565 = CARTESIAN_POINT ( 'NONE',  ( 1.300000000000000044, -0.7216878364870317197, 1.250000000000000000 ) ) ;
#12566 = CARTESIAN_POINT ( 'NONE',  ( 4.898587196589413815E-16, 2.700915433685006750, 35.11257424290206330 ) ) ;
#12567 = CARTESIAN_POINT ( 'NONE',  ( -4.243569643749997233, -23.43122440117877048, -13.45326646829115980 ) ) ;
#12568 = EDGE_LOOP ( 'NONE', ( #9721, #2722, #1120, #10166 ) ) ;
#12569 = CARTESIAN_POINT ( 'NONE',  ( -10.00000000000000000, 23.19999999999999574, 2.499999999999998224 ) ) ;
#12570 = CARTESIAN_POINT ( 'NONE',  ( -3.999999999999997335, -19.59411752552460584, -7.728137727606295471 ) ) ;
#12571 = CARTESIAN_POINT ( 'NONE',  ( -3.500000000000000444, 37.99680007765647360, 0.05647727720536892260 ) ) ;
#12572 = ORIENTED_EDGE ( 'NONE', *, *, #8970, .F. ) ;
#12573 = CARTESIAN_POINT ( 'NONE',  ( 4.000000000000000888, -25.46505466581989907, -12.08638699514879455 ) ) ;
#12574 =( NAMED_UNIT ( * ) SI_UNIT ( $, .STERADIAN. ) SOLID_ANGLE_UNIT ( ) );
#12575 = CARTESIAN_POINT ( 'NONE',  ( -1.444289557196047014, 15.99680007765647716, -4.262301884875704161 ) ) ;
#12576 = FACE_OUTER_BOUND ( 'NONE', #3, .T. ) ;
#12577 = CARTESIAN_POINT ( 'NONE',  ( 1.497042530366522461, 38.62819992234354771, 2.161531897785029965 ) ) ;
#12578 = EDGE_LOOP ( 'NONE', ( #1655, #17930 ) ) ;
#12579 = CARTESIAN_POINT ( 'NONE',  ( 4.243569643749997233, -27.60643051157189731, -10.87309852930384935 ) ) ;
#12580 = CARTESIAN_POINT ( 'NONE',  ( 0.05938372350929014415, 24.87180007765647716, 4.731580009072201776 ) ) ;
#12581 = VERTEX_POINT ( 'NONE', #16817 ) ;
#12582 = ADVANCED_FACE ( 'NONE', ( #1235 ), #1413, .T. ) ;
#12583 = DIRECTION ( 'NONE',  ( 0.000000000000000000, 0.000000000000000000, -1.000000000000000000 ) ) ;
#12584 = CARTESIAN_POINT ( 'NONE',  ( 4.299564228933482956E-15, -20.83337215778458074, -12.44544603592020771 ) ) ;
#12585 = EDGE_CURVE ( 'NONE', #3578, #16574, #4089, .T. ) ;
#12586 = DIRECTION ( 'NONE',  ( 0.000000000000000000, -0.8660254037844387076, 0.5000000000000001110 ) ) ;
#12587 = CARTESIAN_POINT ( 'NONE',  ( -8.500000000000005329, 0.000000000000000000, -20.49999999999999645 ) ) ;
#12588 = CARTESIAN_POINT ( 'NONE',  ( -5.330712181944245322E-15, -27.07529864955322552, -5.843073507603255834 ) ) ;
#12589 = ORIENTED_EDGE ( 'NONE', *, *, #15002, .F. ) ;
#12590 = CARTESIAN_POINT ( 'NONE',  ( -8.500000000000010658, 13.00000000000000178, 18.34999999999999432 ) ) ;
#12591 = ORIENTED_EDGE ( 'NONE', *, *, #6035, .T. ) ;
#12592 = CARTESIAN_POINT ( 'NONE',  ( 4.000000000000003553, -23.29368553998883229, -13.01166841327030710 ) ) ;
#12593 = DIRECTION ( 'NONE',  ( 1.000000000000000000, 0.000000000000000000, 0.000000000000000000 ) ) ;
#12594 =( NAMED_UNIT ( * ) SI_UNIT ( $, .STERADIAN. ) SOLID_ANGLE_UNIT ( ) );
#12595 = CARTESIAN_POINT ( 'NONE',  ( -2.829195390882724315, 16.62819992234354061, 3.793023760679264722 ) ) ;
#12596 = CARTESIAN_POINT ( 'NONE',  ( 3.500000000000000444, 23.25319992234354416, 0.05647727720529520379 ) ) ;
#12597 = CARTESIAN_POINT ( 'NONE',  ( -1.999999999999996225, -23.31572046977624169, -15.05629650786418772 ) ) ;
#12598 = CARTESIAN_POINT ( 'NONE',  ( 2.055738996568313048, 31.99680007765648426, 1.423772053676023441 ) ) ;
#12599 = CARTESIAN_POINT ( 'NONE',  ( -3.673772985318163098, 21.75319992234354416, 2.599342558261029001 ) ) ;
#12600 = CARTESIAN_POINT ( 'NONE',  ( 3.999999999999996447, -25.50702127099278371, -8.120003611597617521 ) ) ;
#12601 = ORIENTED_EDGE ( 'NONE', *, *, #6638, .F. ) ;
#12602 = EDGE_CURVE ( 'NONE', #13230, #13289, #14918, .T. ) ;
#12603 = EDGE_CURVE ( 'NONE', #15334, #16170, #9916, .T. ) ;
#12604 = CARTESIAN_POINT ( 'NONE',  ( 2.769796806539087886, -22.38185710306395748, -1.928164938508226234 ) ) ;
#12605 = ADVANCED_FACE ( 'NONE', ( #6868 ), #3911, .F. ) ;
#12606 = CARTESIAN_POINT ( 'NONE',  ( -0.05938372350927861171, 18.62180007765647005, -3.680117784833935701 ) ) ;
#12607 =( BOUNDED_CURVE ( )  B_SPLINE_CURVE ( 2, ( #918, #6918, #8220, #13699, #12573, #18082, #5531, #13969, #6830 ),
 .UNSPECIFIED., .F., .F. ) 
 B_SPLINE_CURVE_WITH_KNOTS ( ( 3, 2, 2, 2, 3 ),
 ( 0.1982758620689655249, 0.2011494252873563260, 0.2068965517241379282, 0.2126436781609195303, 0.2155172413793103592 ),
 .UNSPECIFIED. ) 
 CURVE ( )  GEOMETRIC_REPRESENTATION_ITEM ( )  RATIONAL_B_SPLINE_CURVE ( ( 0.9330127018922194093, 0.9330127018922194093, 1.000000000000000000, 0.8660254037844387076, 1.000000000000000000, 0.8660254037844387076, 1.000000000000000000, 0.9330127018922189652, 0.9330127018922192983 ) ) 
 REPRESENTATION_ITEM ( '' )  );
#12608 = CIRCLE ( 'NONE', #4614, 6.000000000000000000 ) ;
#12609 = CARTESIAN_POINT ( 'NONE',  ( -3.999999999999997335, -22.43332088546226544, -11.78294034683682057 ) ) ;
#12610 = CARTESIAN_POINT ( 'NONE',  ( -5.330712181944246111E-15, -27.30114437136644767, -6.165614625042047159 ) ) ;
#12611 = VECTOR ( 'NONE', #9058, 1000.000000000000000 ) ;
#12612 = CARTESIAN_POINT ( 'NONE',  ( 3.999999999999996447, 6.938893903907228378E-15, 0.000000000000000000 ) ) ;
#12613 = DIRECTION ( 'NONE',  ( -0.000000000000000000, -1.000000000000000000, -0.000000000000000000 ) ) ;
#12614 = DIRECTION ( 'NONE',  ( -0.000000000000000000, -1.000000000000000000, -0.000000000000000000 ) ) ;
#12615 = ORIENTED_EDGE ( 'NONE', *, *, #14025, .T. ) ;
#12616 = ORIENTED_EDGE ( 'NONE', *, *, #3630, .T. ) ;
#12617 = CARTESIAN_POINT ( 'NONE',  ( -1.027846397803541700, 24.99680007765647716, 3.346150245485522312 ) ) ;
#12618 = CARTESIAN_POINT ( 'NONE',  ( -1.071796769724477238, -25.13965799397821144, -4.647885204373104706 ) ) ;
#12619 = CARTESIAN_POINT ( 'NONE',  ( -3.999999999999997335, -24.24008665996804268, -14.36326928634715649 ) ) ;
#12620 = CARTESIAN_POINT ( 'NONE',  ( 4.000000000000000888, -21.07719492773443193, -5.819873856337981266 ) ) ;
#12621 = CARTESIAN_POINT ( 'NONE',  ( -4.648177544792955347E-16, -30.09673717385520675, -11.72732795437737785 ) ) ;
#12622 = VERTEX_POINT ( 'NONE', #5485 ) ;
#12623 = CARTESIAN_POINT ( 'NONE',  ( -2.798362969681409851, 17.25319992234354416, -2.102939460078765421 ) ) ;
#12624 = CARTESIAN_POINT ( 'NONE',  ( 2.121784821875004390, -19.39496705955529876, -9.824638646973991030 ) ) ;
#12625 = CARTESIAN_POINT ( 'NONE',  ( -2.798362969681365886, 27.74680007765648071, 2.102939460078824929 ) ) ;
#12626 = CARTESIAN_POINT ( 'NONE',  ( 2.798362969681409851, 23.50319992234354416, 2.102939460078764977 ) ) ;
#12627 = DIRECTION ( 'NONE',  ( 1.000000000000000000, 0.000000000000000000, -0.000000000000000000 ) ) ;
#12628 = AXIS2_PLACEMENT_3D ( 'NONE', #13114, #426, #3206 ) ;
#12629 = DIRECTION ( 'NONE',  ( 0.000000000000000000, 0.000000000000000000, 1.000000000000000000 ) ) ;
#12630 = CARTESIAN_POINT ( 'NONE',  ( -4.243569643749997233, -21.91483169757570693, -11.28763325120213068 ) ) ;
#12631 = AXIS2_PLACEMENT_3D ( 'NONE', #2241, #7591, #12041 ) ;
#12632 = LINE ( 'NONE', #2646, #1999 ) ;
#12633 = ADVANCED_FACE ( 'NONE', ( #8353 ), #13865, .T. ) ;
#12634 = DIRECTION ( 'NONE',  ( 0.000000000000000000, 0.000000000000000000, -1.000000000000000000 ) ) ;
#12635 = CARTESIAN_POINT ( 'NONE',  ( 2.399999999999999911, 0.000000000000000000, 0.000000000000000000 ) ) ;
#12636 = AXIS2_PLACEMENT_3D ( 'NONE', #7061, #18322, #14216 ) ;
#12637 = CARTESIAN_POINT ( 'NONE',  ( -2.121784821874996396, -17.02896425960724969, -6.445636464281891520 ) ) ;
#12638 = CARTESIAN_POINT ( 'NONE',  ( -3.000000000000003553, 15.00000000000000711, -0.1687737011545533683 ) ) ;
#12639 = CARTESIAN_POINT ( 'NONE',  ( 0.000000000000000000, 3.000000000000000000, 0.000000000000000000 ) ) ;
#12640 = EDGE_LOOP ( 'NONE', ( #18183, #3946, #695, #3487 ) ) ;
#12641 = CARTESIAN_POINT ( 'NONE',  ( -2.055738996568313048, 35.74680007765648071, -1.423772053676023441 ) ) ;
#12642 = CARTESIAN_POINT ( 'NONE',  ( 4.299564228933482956E-15, -16.96173121241504944, -6.916169736969493442 ) ) ;
#12643 = CARTESIAN_POINT ( 'NONE',  ( 1.027846397803542144, 38.74680007765647360, -3.346150245485522312 ) ) ;
#12644 = CARTESIAN_POINT ( 'NONE',  ( -10.00530551168418825, -9.915183271925439357, 7.312645477306290331 ) ) ;
#12645 = ORIENTED_EDGE ( 'NONE', *, *, #947, .F. ) ;
#12646 = CARTESIAN_POINT ( 'NONE',  ( -2.121784821875005722, -22.99602307520341427, -2.153009282964420290 ) ) ;
#12647 = CARTESIAN_POINT ( 'NONE',  ( 0.05938372350927906274, 34.87180007765645939, 3.680117784833935701 ) ) ;
#12648 = AXIS2_PLACEMENT_3D ( 'NONE', #9065, #9587, #4807 ) ;
#12649 = CIRCLE ( 'NONE', #7013, 0.1999999999999987899 ) ;
#12650 = EDGE_CURVE ( 'NONE', #16492, #3217, #11, .T. ) ;
#12651 = FACE_OUTER_BOUND ( 'NONE', #13262, .T. ) ;
#12652 = CARTESIAN_POINT ( 'NONE',  ( 8.000000000000005329, 34.19999999999999574, 2.499999999999997780 ) ) ;
#12653 = EDGE_CURVE ( 'NONE', #9649, #17767, #7644, .T. ) ;
#12654 = CARTESIAN_POINT ( 'NONE',  ( 4.000000000000000888, -26.43296490145733557, -13.46870606887970645 ) ) ;
#12655 = CARTESIAN_POINT ( 'NONE',  ( 20.00000000000000355, 0.000000000000000000, 0.000000000000000000 ) ) ;
#12656 = CARTESIAN_POINT ( 'NONE',  ( -4.243569643750005227, -28.69264088791166856, -12.42436771317613875 ) ) ;
#12657 = ORIENTED_EDGE ( 'NONE', *, *, #16764, .F. ) ;
#12658 = DIRECTION ( 'NONE',  ( 0.000000000000000000, 0.000000000000000000, -1.000000000000000000 ) ) ;
#12659 = CARTESIAN_POINT ( 'NONE',  ( 4.713407268011036227E-15, -18.51971333421491295, -10.22004743043051000 ) ) ;
#12660 = CARTESIAN_POINT ( 'NONE',  ( -2.518350579753628526, 15.62180007765648071, -0.7558219633769075463 ) ) ;
#12661 = PRODUCT_DEFINITION_CONTEXT ( 'detailed design', #4758, 'design' ) ;
#12662 = AXIS2_PLACEMENT_3D ( 'NONE', #17604, #16008, #3300 ) ;
#12663 = ORIENTED_EDGE ( 'NONE', *, *, #8190, .T. ) ;
#12664 = CARTESIAN_POINT ( 'NONE',  ( -10.00000000000000000, 38.59999999999999432, 2.499999999999998224 ) ) ;
#12665 = CARTESIAN_POINT ( 'NONE',  ( 4.481649420246397675, 38.37819992234354061, 1.518615910253363177 ) ) ;
#12666 = UNCERTAINTY_MEASURE_WITH_UNIT (LENGTH_MEASURE( 1.000000000000000082E-05 ), #17600, 'distance_accuracy_value', 'NONE');
#12667 = CARTESIAN_POINT ( 'NONE',  ( -0.7188294034286550893, 32.50319992234354771, -2.395093729190349130 ) ) ;
#12668 = EDGE_LOOP ( 'NONE', ( #18275, #15471, #8038, #16154 ) ) ;
#12669 = CARTESIAN_POINT ( 'NONE',  ( 4.243569643749997233, -27.86453990792986701, -11.24171694923389531 ) ) ;
#12670 = CARTESIAN_POINT ( 'NONE',  ( 0.05938372350929014415, 37.37180007765647360, 4.731580009072201776 ) ) ;
#12671 = VECTOR ( 'NONE', #6808, 1000.000000000000000 ) ;
#12672 = ORIENTED_EDGE ( 'NONE', *, *, #10179, .F. ) ;
#12673 = AXIS2_PLACEMENT_3D ( 'NONE', #7990, #1054, #6608 ) ;
#12674 = FILL_AREA_STYLE ('',( #15741 ) ) ;
#12676 = EDGE_CURVE ( 'NONE', #2215, #9856, #14103, .T. ) ;
#12675 = VECTOR ( 'NONE', #4349, 1000.000000000000000 ) ;
#12677 = AXIS2_PLACEMENT_3D ( 'NONE', #3374, #16265, #17765 ) ;
#12678 =( NAMED_UNIT ( * ) SI_UNIT ( $, .STERADIAN. ) SOLID_ANGLE_UNIT ( ) );
#12679 = CARTESIAN_POINT ( 'NONE',  ( 1.071796769724495224, -17.94116814877132526, -8.314950645356326220 ) ) ;
#12680 = DIRECTION ( 'NONE',  ( -0.000000000000000000, -1.000000000000000000, -0.000000000000000000 ) ) ;
#12681 = CARTESIAN_POINT ( 'NONE',  ( 2.121784821875004390, -19.68534013045801956, -10.23933436939529606 ) ) ;
#12682 = EDGE_LOOP ( 'NONE', ( #13730, #9706, #7760, #11465 ) ) ;
#12683 = FACE_OUTER_BOUND ( 'NONE', #10091, .T. ) ;
#12684 = ORIENTED_EDGE ( 'NONE', *, *, #207, .T. ) ;
#12685 = CARTESIAN_POINT ( 'NONE',  ( -5.279047395330986450E-15, -28.02253625933941095, -7.686213421056266704 ) ) ;
#12686 = DIRECTION ( 'NONE',  ( -0.000000000000000000, -0.5735764363510414965, -0.8191520442889950182 ) ) ;
#12687 = PRESENTATION_STYLE_ASSIGNMENT (( #5217 ) ) ;
#12688 = CARTESIAN_POINT ( 'NONE',  ( -4.499999999999999112, 22.00319992234354061, -0.05647727720528529505 ) ) ;
#12689 = CARTESIAN_POINT ( 'NONE',  ( -1.027846397803611866, 22.50319992234354416, -3.346150245485499219 ) ) ;
#12690 = TOROIDAL_SURFACE ( 'NONE', #15372, 9.000000000000001776, 0.9999999999999991118 ) ;
#12691 = CARTESIAN_POINT ( 'NONE',  ( -5.279047395330986450E-15, -30.60363022291909729, -11.37239762035674495 ) ) ;
#12692 = CARTESIAN_POINT ( 'NONE',  ( -1.989345975306426206, 37.74680007765647360, 1.515154207786343799 ) ) ;
#12693 = CARTESIAN_POINT ( 'NONE',  ( -1.336863392178569088, 30.00319992234354416, -4.297206761780648421 ) ) ;
#12694 = ADVANCED_BREP_SHAPE_REPRESENTATION ( '', ( #1642, #16940 ), #3923 ) ;
#12695 = CARTESIAN_POINT ( 'NONE',  ( 4.000000000000003553, -21.42239241568861274, -10.33918486777069745 ) ) ;
#12696 = ORIENTED_EDGE ( 'NONE', *, *, #4861, .T. ) ;
#12697 = CARTESIAN_POINT ( 'NONE',  ( 4.000000000000003553, -18.90582580190336515, -6.745155274459496475 ) ) ;
#12698 = CARTESIAN_POINT ( 'NONE',  ( 3.500000000000000444, 24.24680007765647716, -0.05647727720536935281 ) ) ;
#12699 = CARTESIAN_POINT ( 'NONE',  ( -6.804503976930308617, -11.93919774785484300, 12.87494948068499134 ) ) ;
#12700 = AXIS2_PLACEMENT_3D ( 'NONE', #6185, #16303, #17624 ) ;
#12701 = CARTESIAN_POINT ( 'NONE',  ( 4.243569643749997233, -25.50929166616339927, -7.878073867372210159 ) ) ;
#12702 = AXIS2_PLACEMENT_3D ( 'NONE', #10654, #3251, #17362 ) ;
#12703 = CARTESIAN_POINT ( 'NONE',  ( 3.673772985318219053, 19.49680007765647005, 2.599342558260951730 ) ) ;
#12704 = CARTESIAN_POINT ( 'NONE',  ( -5.577813053751546416E-15, -23.12778347219005681, -1.774630616266089866 ) ) ;
#12705 = CARTESIAN_POINT ( 'NONE',  ( 0.000000000000000000, 13.00000000000000178, 6.000000000000000888 ) ) ;
#12706 = CARTESIAN_POINT ( 'NONE',  ( -1.071796769724496334, -20.04751726799184297, -11.32312894147414539 ) ) ;
#12707 = VERTEX_POINT ( 'NONE', #5571 ) ;
#12708 = ORIENTED_EDGE ( 'NONE', *, *, #8300, .T. ) ;
#12709 = CARTESIAN_POINT ( 'NONE',  ( 1.027846397803542144, 23.74680007765647716, -3.346150245485522312 ) ) ;
#12710 = CARTESIAN_POINT ( 'NONE',  ( 3.579096709490575479E-14, -23.06325612239561451, -1.682476010276811040 ) ) ;
#12711 = EDGE_CURVE ( 'NONE', #8864, #17673, #16908, .T. ) ;
#12712 = DIRECTION ( 'NONE',  ( 0.000000000000000000, 0.000000000000000000, -1.000000000000000000 ) ) ;
#12713 = CARTESIAN_POINT ( 'NONE',  ( 2.000000000000004441, -20.00331654984898577, -10.32569345209524414 ) ) ;
#12714 = ORIENTED_EDGE ( 'NONE', *, *, #2483, .F. ) ;
#12715 = CARTESIAN_POINT ( 'NONE',  ( -2.798362969681409851, 19.75319992234354416, -2.102939460078765421 ) ) ;
#12716 = AXIS2_PLACEMENT_3D ( 'NONE', #6629, #12274, #5232 ) ;
#12717 = ADVANCED_FACE ( 'NONE', ( #17002 ), #7351, .F. ) ;
#12718 = CARTESIAN_POINT ( 'NONE',  ( 2.121784821874994176, -26.27616332058593684, -6.837535036242106123 ) ) ;
#12719 = CARTESIAN_POINT ( 'NONE',  ( -0.05938372350926768989, 16.12180007765648071, -2.628655560595669183 ) ) ;
#12720 = EDGE_CURVE ( 'NONE', #17541, #15647, #15920, .T. ) ;
#12721 = CIRCLE ( 'NONE', #9449, 2.000000000000001776 ) ;
#12722 = CARTESIAN_POINT ( 'NONE',  ( -2.798362969681409851, 27.25319992234354771, -2.102939460078765421 ) ) ;
#12723 = DIRECTION ( 'NONE',  ( -0.000000000000000000, -1.000000000000000000, -0.000000000000000000 ) ) ;
#12724 = FACE_OUTER_BOUND ( 'NONE', #9714, .T. ) ;
#12725 =( BOUNDED_SURFACE ( )  B_SPLINE_SURFACE ( 3, 2, ( 
 ( #10218, #12825, #11423, #7445, #14320, #13103, #5780, #7347, #13008, #417, #3194, #7251, #6055, #8833, #3007, #4299, #10314, #15997, #11520, #14607, #1909, #12740, #11335, #15617, #2918, #8552, #14227, #1530, #17113, #4389, #11800, #6245, #13383, #16274, #698, #17775, #16455, #12170, #509, #13192, #6344, #16093, #6151, #9026, #2094, #17497, #3474, #14978, #6431, #9118, #6521, #11987, #3385, #3736, #17681, #13473, #17861, #5125, #2275, #10782, #9387, #14797, #3567, #10414, #4762, #9213, #4945, #14703, #12076, #7904, #14891, #2001, #7627, #13292, #7722, #605, #11895, #15064, #10600, #2188, #3652, #7816, #784, #17594, #4857, #5037, #10508, #7539, #10693, #16366, #16177, #9299, #13559, #876, #12351, #2459, #13937, #9574, #12625, #15434, #6967, #8180, #17947, #2368, #18315, #18226, #18042, #1335, #1150, #5495, #6791, #16738, #6617, #13652, #2549, #16552, #6696, #9479, #9753, #1245, #2731, #15253, #12260, #11141, #15154, #7998, #8089, #972, #5219, #14024, #10872, #11232, #5315, #4102, #3828, #18138, #13751, #9659, #1061, #8278, #8364, #10967, #4196, #5406, #16649, #9843, #13840, #3922, #12446, #11057, #4015, #5586, #15338, #2637, #6879, #16831, #16920, #12537, #23, #8444, #13080, #17192, #15692, #17288, #4465, #7235, #3082, #12893, #14492, #398, #6034, #8622, #17378, #113, #5766, #17013, #11403, #2816, #7423, #200, #2990, #7054, #5943, #1600, #11686, #11592, #2901, #17095, #5851, #15599, #14299, #14388, #8535, #11497, #4643, #4284, #10102, #15519, #4558, #14114, #4367 ),
 ( #10017, #1427, #10198, #1791, #15785, #12719, #5674, #11319, #12987, #7145, #9928, #8715, #301, #1692, #7327, #14206, #1511, #15877, #12807, #3174, #8812, #855, #16069, #6501, #3364, #9281, #4743, #486, #13268, #675, #11875, #3545, #10391, #9009, #17753, #17567, #12056, #6128, #1889, #7702, #14584, #2256, #2165, #16252, #17474, #9189, #16161, #4839, #1980, #14684, #14871, #10487, #7881, #5014, #14961, #3453, #7520, #10296, #13538, #7797, #7607, #12145, #9094, #13454, #14776, #6322, #13172, #3270, #2073, #11780, #585, #10670, #17838, #6226, #15976, #13363, #8907, #11971, #17663, #4925, #10576, #766, #6411, #16340, #3632, #12512, #6677, #6858, #10849, #18113, #2526, #18207, #8255, #12330, #16805, #12422, #2436, #9366, #13913, #9729, #3901, #13998, #8339, #5471, #1313, #2348, #9548, #10763, #11032, #16438, #11116, #15412, #15042, #3804, #10943, #13819, #16626, #15315, #6945, #2707, #3716, #7979, #15226, #13632, #944, #6588, #18016, #12238, #1036, #4075, #3988, #5290, #12598, #8156, #17926, #5102, #1129, #16715, #5198, #16525, #9459, #15132, #8062, #6765, #5383, #13725, #9637, #2615, #1221, #16897, #17165, #277, #8598, #4173, #9816, #14088, #12782, #1399, #5559, #3151, #17071, #2964, #14366, #90, #1577, #5743, #14273, #11383, #10079, #8784, #4533, #11208, #15497, #4344, #8425, #2794, #7027, #9991, #12692, #14180, #7301, #4439, #1487, #17260, #15666, #18369, #14465, #7214, #5826, #10175, #15853, #12961, #1769, #7399, #7121, #12868, #5651, #11293, #176, #11471, #16985 ),
 ( #1666, #4262, #8507, #15758, #9905, #3058, #8690, #15577, #5920, #18286, #2877, #11565, #13059, #14848, #11664, #3339, #16047, #6296, #8985, #9167, #4816, #3431, #13242, #13431, #11851, #14658, #14940, #745, #17643, #1958, #17449, #6104, #9255, #17547, #2232, #2140, #11756, #7493, #3606, #370, #7771, #561, #16226, #10464, #16142, #6203, #16319, #6389, #3246, #4991, #9072, #6009, #13342, #4900, #10648, #1862, #14751, #13151, #2048, #10551, #462, #12033, #11949, #17725, #7584, #4621, #3519, #4718, #17356, #10368, #10269, #15949, #8884, #14562, #7680, #652, #9617, #7858, #5266, #13516, #15204, #9342, #13793, #15291, #13608, #9700, #16779, #12485, #831, #6472, #1015, #16412, #12124, #15021, #2411, #17818, #3782, #2591, #6743, #9433, #6835, #6656, #3696, #4049, #12303, #1103, #18178, #5447, #8224, #11094, #15385, #15108, #3876, #10739, #5079, #16600, #17995, #2320, #12398, #13888, #9523, #7951, #922, #6564, #8042, #12215, #17902, #5172, #10921, #2504, #3965, #13703, #8132, #10826, #16503, #18090, #5360, #11007, #16687, #1199, #9796, #14250, #8484, #9884, #12667, #2774, #1552, #15556, #12937, #15734, #7279, #14156, #18265, #2684, #249, #154, #18356, #1641, #1467, #5805, #7098, #17050, #6921, #13977, #2851, #16870, #7004, #4415, #11544, #8404, #17235, #14061, #5894, #15477, #11182, #5630, #11360, #4240, #7191, #1374, #11273, #10058, #12761, #3035, #16962, #15643, #65, #8666, #11448, #5720, #14343, #9967, #4321, #12577, #17138, #4509, #2943, #10151, #8316, #1290, #5535 ),
 ( #4149, #8578, #12848, #3312, #6178, #8955, #7649, #11638, #12263, #1936, #3407, #14819, #7999, #4877, #13653, #17948, #17425, #11827, #348, #14437, #17523, #14633, #1739, #14725, #16201, #4786, #7372, #13033, #17332, #10341, #4595, #3126, #974, #7559, #532, #11921, #16021, #10439, #10245, #5986, #13215, #15924, #6618, #13315, #9049, #3222, #2024, #16115, #4691, #7470, #8858, #629, #6267, #5220, #10528, #2118, #17617, #14537, #15830, #8761, #3494, #13128, #1833, #9139, #437, #6076, #11729, #15155, #3831, #11058, #6697, #15255, #12626, #1428, #16650, #7055, #3924, #9845, #5317, #1062, #13841, #1246, #12447, #4103, #10969, #9575, #18316, #18140, #5588, #2551, #5496, #8280, #11234, #14026, #5408, #4197, #18228, #8181, #2462, #1336, #15520, #9661, #12722, #14115, #16922, #24, #8090, #15339, #16553, #16833, #9480, #2818, #8445, #13753, #1152, #16740, #6881, #4016, #2732, #10873, #12352, #18043, #6794, #2638, #13938, #12538, #11142, #9755, #15435, #8365, #6968, #4560, #7237, #4644, #4466, #202, #9930, #1601, #13082, #10199, #12894, #10297, #10105, #1513, #1890, #15788, #11594, #15977, #3273, #399, #8910, #7522, #5853, #1694, #8536, #4285, #14389, #3083, #15601, #15878, #6037, #7329, #2902, #14209, #7146, #11498, #12808, #11320, #14587, #8716, #12989, #1792, #17194, #303, #114, #5767, #5945, #11405, #13175, #3175, #17291, #17097, #8813, #14494, #7425, #15694, #4368, #11688, #17379, #5675, #17014, #10018, #2992, #8624, #14301, #5104, #16341, #10489, #17840, #17664, #3634 ),
 ( #9282, #10578, #16254, #11972, #3717, #7882, #9010, #10764, #4926, #15044, #767, #5016, #16439, #7608, #3546, #13269, #9191, #14962, #586, #13540, #12057, #856, #7704, #10394, #2257, #6228, #6129, #11877, #487, #16071, #12148, #4745, #9367, #3455, #6502, #11781, #14872, #17475, #7798, #1982, #6412, #2349, #17570, #7980, #2167, #14686, #3366, #6324, #4840, #13455, #17755, #10672, #16162, #9096, #14777, #2074, #13364, #677, #12599, #12423, #11118, #18115, #9639, #17927, #6591, #13820, #9460, #18018, #15413, #4175, #1037, #9817, #6678, #18288, #8065, #3805, #16628, #3991, #15228, #6859, #13727, #12331, #2709, #2528, #8340, #5291, #8256, #11034, #14000, #16806, #8157, #6946, #2616, #10944, #5200, #4078, #5561, #5384, #15499, #16898, #1314, #2795, #10850, #16717, #946, #1223, #12239, #11209, #13634, #16527, #3902, #1130, #15317, #6766, #5472, #15134, #2437, #9550, #13914, #12514, #18208, #9730, #9906, #2968, #12693, #4346, #15855, #7303, #9994, #7401, #7216, #4263, #4623, #12870, #14368, #13061, #372, #3153, #6013, #10271, #15669, #4441, #11294, #7030, #17167, #178, #1, #12964, #8786, #10082, #5652, #16987, #15578, #8600, #2878, #14089, #11666, #5828, #11474, #4536, #14276, #15760, #8509, #14183, #3060, #1488, #17358, #279, #1668, #7123, #5922, #1580, #8692, #92, #12784, #11568, #17263, #15952, #14470, #8426, #10178, #5744, #1400, #11384, #17073, #1771, #747, #13244, #2234, #2051, #6392, #7682, #17645, #7495, #14565, #3433, #17452, #7586, #4994, #12126, #8988 ),
 ( #3522, #7773, #13519, #10370, #655, #16050, #13344, #12035, #3341, #10650, #14850, #3609, #10467, #13153, #17727, #14661, #8886, #1960, #3248, #464, #14943, #6106, #17820, #6205, #16321, #1865, #6298, #11758, #10553, #4720, #9169, #9257, #564, #5081, #11952, #11853, #10741, #9074, #17550, #4903, #16228, #2143, #7861, #4818, #13434, #16144, #833, #6474, #14753, #924, #9344, #13980, #18093, #16604, #18181, #5364, #8136, #3969, #13798, #15388, #1294, #6925, #9527, #18268, #1018, #6659, #17906, #12307, #3698, #8319, #1106, #3879, #7953, #6838, #2508, #12580, #12489, #3784, #17998, #6746, #16505, #15207, #15294, #9437, #12402, #5538, #5174, #11011, #16415, #5450, #15023, #5269, #10924, #9620, #16690, #11097, #2595, #8228, #13891, #16783, #1202, #4052, #2323, #9704, #2687, #13610, #15110, #6567, #12217, #2413, #10829, #8044, #13705, #8581, #11185, #12941, #9799, #1471, #14159, #4419, #7102, #7282, #2947, #1557, #11363, #11547, #9970, #12764, #13036, #17238, #15738, #69, #15560, #4244, #7376, #15646, #351, #252, #9887, #5634, #1745, #16875, #5898, #17054, #14346, #14254, #7194, #4325, #14441, #4512, #1378, #3129, #12851, #4152, #11451, #3040, #8764, #18361, #158, #11276, #5809, #8669, #16966, #10155, #10061, #15833, #5723, #2777, #1645, #2854, #15481, #8487, #8408, #14064, #7007, #12670, #17141, #8958, #7750, #5989, #3410, #11641, #13319, #7473, #11925, #13410, #11732, #7841, #9052, #1836, #13493, #11831, #10345, #16118, #14728, #2028, #722, #3225, #7652, #16025, #3498 ),
 ( #13131, #2213, #10442, #17620, #4969, #16299, #6368, #3586, #17336, #7562, #633, #8863, #4598, #6271, #4790, #10248, #4880, #12009, #10531, #15927, #14540, #441, #535, #6081, #13219, #16205, #17428, #4694, #17705, #6181, #10625, #3315, #9144, #14823, #9236, #2121, #17527, #14921, #14636, #1939, #5060, #3948, #5431, #17975, #9681, #4034, #13869, #15366, #16391, #5243, #6455, #6722, #12102, #8205, #11077, #10715, #17883, #6639, #9503, #12285, #10991, #2664, #16761, #17799, #3679, #10900, #9325, #14999, #2297, #13677, #7930, #15086, #1175, #18067, #2392, #18160, #16577, #13586, #8298, #3856, #12377, #808, #902, #6816, #6543, #12195, #8023, #15179, #5152, #10809, #2484, #8114, #16481, #5339, #12466, #13773, #3762, #9411, #997, #1085, #16669, #9599, #15274, #2573, #17035, #10038, #14135, #15623, #9779, #5516, #11342, #18247, #5878, #5786, #1536, #2753, #7171, #1448, #2837, #5610, #14046, #12831, #8466, #11525, #8648, #229, #7078, #11161, #13957, #17217, #11428, #11256, #12917, #12746, #17118, #47, #9951, #16853, #6904, #5701, #15456, #18339, #15715, #4489, #1355, #10131, #6986, #15812, #8383, #4130, #16944, #4304, #7257, #2924, #4219, #12647, #4398, #3109, #8557, #1269, #12562, #14326, #9865, #15539, #14233, #134, #3015, #1623, #1915, #6156, #1719, #4579, #1815, #6059, #7450, #3294, #17502, #11805, #14414, #8739, #11711, #11619, #328, #17313, #13108, #5964, #422, #4766, #14613, #17405, #10417, #4668, #10224, #7355, #10321, #7543, #13015, #15902, #3199, #8839, #14516 ) ),
 .UNSPECIFIED., .T., .F., .F. ) 
 B_SPLINE_SURFACE_WITH_KNOTS ( ( 4, 3, 4 ),
 ( 3, 2, 2, 2, 2, 2, 2, 2, 2, 2, 2, 2, 2, 2, 2, 2, 2, 2, 2, 2, 2, 2, 2, 2, 2, 2, 2, 2, 2, 2, 2, 2, 2, 2, 2, 2, 2, 2, 2, 2, 2, 2, 2, 2, 2, 2, 2, 2, 2, 2, 2, 2, 2, 2, 2, 2, 2, 2, 2, 2, 2, 2, 2, 2, 2, 2, 2, 2, 2, 2, 2, 2, 2, 2, 2, 2, 2, 2, 2, 2, 2, 2, 2, 2, 2, 2, 2, 2, 2, 2, 2, 2, 2, 2, 2, 2, 2, 2, 2, 2, 3 ),
 ( 0.000000000000000000, 0.5000000000000000000, 1.000000000000000000 ),
 ( 0.000000000000000000, 0.01000000000000000021, 0.02000000000000000042, 0.02999999999999999889, 0.04000000000000000083, 0.05000000000000000278, 0.05999999999999999778, 0.07000000000000000666, 0.08000000000000000167, 0.08999999999999999667, 0.1000000000000000056, 0.1100000000000000006, 0.1199999999999999956, 0.1300000000000000044, 0.1400000000000000133, 0.1499999999999999944, 0.1600000000000000033, 0.1700000000000000122, 0.1799999999999999933, 0.1900000000000000022, 0.2000000000000000111, 0.2099999999999999922, 0.2200000000000000011, 0.2300000000000000100, 0.2399999999999999911, 0.2500000000000000000, 0.2600000000000000089, 0.2700000000000000178, 0.2800000000000000266, 0.2899999999999999800, 0.2999999999999999889, 0.3099999999999999978, 0.3200000000000000067, 0.3300000000000000155, 0.3400000000000000244, 0.3499999999999999778, 0.3599999999999999867, 0.3699999999999999956, 0.3800000000000000044, 0.3900000000000000133, 0.4000000000000000222, 0.4099999999999999756, 0.4199999999999999845, 0.4299999999999999933, 0.4400000000000000022, 0.4500000000000000111, 0.4600000000000000200, 0.4699999999999999734, 0.4799999999999999822, 0.4899999999999999911, 0.5000000000000000000, 0.5100000000000000089, 0.5200000000000000178, 0.5300000000000000266, 0.5400000000000000355, 0.5500000000000000444, 0.5600000000000000533, 0.5699999999999999512, 0.5799999999999999600, 0.5899999999999999689, 0.5999999999999999778, 0.6099999999999999867, 0.6199999999999999956, 0.6300000000000000044, 0.6400000000000000133, 0.6500000000000000222, 0.6600000000000000311, 0.6700000000000000400, 0.6800000000000000488, 0.6899999999999999467, 0.6999999999999999556, 0.7099999999999999645, 0.7199999999999999734, 0.7299999999999999822, 0.7399999999999999911, 0.7500000000000000000, 0.7600000000000000089, 0.7700000000000000178, 0.7800000000000000266, 0.7900000000000000355, 0.8000000000000000444, 0.8100000000000000533, 0.8199999999999999512, 0.8299999999999999600, 0.8399999999999999689, 0.8499999999999999778, 0.8599999999999999867, 0.8699999999999999956, 0.8800000000000000044, 0.8900000000000000133, 0.9000000000000000222, 0.9100000000000000311, 0.9200000000000000400, 0.9300000000000000488, 0.9399999999999999467, 0.9499999999999999556, 0.9599999999999999645, 0.9699999999999999734, 0.9799999999999999822, 0.9899999999999999911, 1.000000000000000000 ),
 .UNSPECIFIED. ) 
 GEOMETRIC_REPRESENTATION_ITEM ( )  RATIONAL_B_SPLINE_SURFACE ( (
 ( 1.000000000000000000, 0.9510565162951535312, 1.000000000000000000, 0.9510565162951535312, 1.000000000000000000, 0.9510565162951535312, 1.000000000000000000, 0.9510565162951535312, 1.000000000000000000, 0.9510565162951535312, 1.000000000000000000, 0.9510565162951535312, 1.000000000000000000, 0.9510565162951535312, 1.000000000000000000, 0.9510565162951535312, 1.000000000000000000, 0.9510565162951535312, 1.000000000000000000, 0.9510565162951535312, 1.000000000000000000, 0.9510565162951535312, 1.000000000000000000, 0.9510565162951535312, 1.000000000000000000, 0.9510565162951535312, 1.000000000000000000, 0.9510565162951535312, 1.000000000000000000, 0.9510565162951535312, 1.000000000000000000, 0.9510565162951535312, 1.000000000000000000, 0.9510565162951535312, 1.000000000000000000, 0.9510565162951535312, 1.000000000000000000, 0.9510565162951535312, 1.000000000000000000, 0.9510565162951535312, 1.000000000000000000, 0.9510565162951535312, 1.000000000000000000, 0.9510565162951535312, 1.000000000000000000, 0.9510565162951535312, 1.000000000000000000, 0.9510565162951535312, 1.000000000000000000, 0.9510565162951535312, 1.000000000000000000, 0.9510565162951535312, 1.000000000000000000, 0.9510565162951535312, 1.000000000000000000, 0.9510565162951535312, 1.000000000000000000, 0.9510565162951535312, 1.000000000000000000, 0.9510565162951535312, 1.000000000000000000, 0.9510565162951535312, 1.000000000000000000, 0.9510565162951535312, 1.000000000000000000, 0.9510565162951535312, 1.000000000000000000, 0.9510565162951535312, 1.000000000000000000, 0.9510565162951535312, 1.000000000000000000, 0.9510565162951535312, 1.000000000000000000, 0.9510565162951535312, 1.000000000000000000, 0.9510565162951535312, 1.000000000000000000, 0.9510565162951535312, 1.000000000000000000, 0.9510565162951535312, 1.000000000000000000, 0.9510565162951535312, 1.000000000000000000, 0.9510565162951535312, 1.000000000000000000, 0.9510565162951535312, 1.000000000000000000, 0.9510565162951535312, 1.000000000000000000, 0.9510565162951535312, 1.000000000000000000, 0.9510565162951535312, 1.000000000000000000, 0.9510565162951535312, 1.000000000000000000, 0.9510565162951535312, 1.000000000000000000, 0.9510565162951535312, 1.000000000000000000, 0.9510565162951535312, 1.000000000000000000, 0.9510565162951535312, 1.000000000000000000, 0.9510565162951535312, 1.000000000000000000, 0.9510565162951535312, 1.000000000000000000, 0.9510565162951535312, 1.000000000000000000, 0.9510565162951535312, 1.000000000000000000, 0.9510565162951535312, 1.000000000000000000, 0.9510565162951535312, 1.000000000000000000, 0.9510565162951535312, 1.000000000000000000, 0.9510565162951535312, 1.000000000000000000, 0.9510565162951535312, 1.000000000000000000, 0.9510565162951535312, 1.000000000000000000, 0.9510565162951535312, 1.000000000000000000, 0.9510565162951535312, 1.000000000000000000, 0.9510565162951535312, 1.000000000000000000, 0.9510565162951535312, 1.000000000000000000, 0.9510565162951535312, 1.000000000000000000, 0.9510565162951535312, 1.000000000000000000, 0.9510565162951535312, 1.000000000000000000, 0.9510565162951535312, 1.000000000000000000, 0.9510565162951535312, 1.000000000000000000, 0.9510565162951535312, 1.000000000000000000, 0.9510565162951535312, 1.000000000000000000, 0.9510565162951535312, 1.000000000000000000, 0.9510565162951535312, 1.000000000000000000, 0.9510565162951535312, 1.000000000000000000, 0.9510565162951535312, 1.000000000000000000, 0.9510565162951535312, 1.000000000000000000, 0.9510565162951535312, 1.000000000000000000, 0.9510565162951535312, 1.000000000000000000, 0.9510565162951535312, 1.000000000000000000, 0.9510565162951535312, 1.000000000000000000, 0.9510565162951535312, 1.000000000000000000, 0.9510565162951535312, 1.000000000000000000, 0.9510565162951535312, 1.000000000000000000, 0.9510565162951535312, 1.000000000000000000, 0.9510565162951535312, 1.000000000000000000, 0.9510565162951535312, 1.000000000000000000, 0.9510565162951535312, 1.000000000000000000, 0.9510565162951535312, 1.000000000000000000, 0.9510565162951535312, 1.000000000000000000, 0.9510565162951535312, 1.000000000000000000, 0.9510565162951535312, 1.000000000000000000, 0.9510565162951535312, 1.000000000000000000, 0.9510565162951535312, 1.000000000000000000, 0.9510565162951535312, 1.000000000000000000, 0.9510565162951535312, 1.000000000000000000, 0.9510565162951535312, 1.000000000000000000, 0.9510565162951535312, 1.000000000000000000, 0.9510565162951535312, 1.000000000000000000, 0.9510565162951535312, 1.000000000000000000),
 ( 0.3333333333333333703, 0.3170188387650512141, 0.3333333333333333703, 0.3170188387650512141, 0.3333333333333333703, 0.3170188387650512141, 0.3333333333333333703, 0.3170188387650512141, 0.3333333333333333703, 0.3170188387650512141, 0.3333333333333333703, 0.3170188387650512141, 0.3333333333333333703, 0.3170188387650512141, 0.3333333333333333703, 0.3170188387650512141, 0.3333333333333333703, 0.3170188387650512141, 0.3333333333333333703, 0.3170188387650512141, 0.3333333333333333703, 0.3170188387650512141, 0.3333333333333333703, 0.3170188387650512141, 0.3333333333333333703, 0.3170188387650512141, 0.3333333333333333703, 0.3170188387650512141, 0.3333333333333333703, 0.3170188387650512141, 0.3333333333333333703, 0.3170188387650512141, 0.3333333333333333703, 0.3170188387650512141, 0.3333333333333333703, 0.3170188387650512141, 0.3333333333333333703, 0.3170188387650512141, 0.3333333333333333703, 0.3170188387650512141, 0.3333333333333333703, 0.3170188387650512141, 0.3333333333333333703, 0.3170188387650512141, 0.3333333333333333703, 0.3170188387650512141, 0.3333333333333333703, 0.3170188387650512141, 0.3333333333333333703, 0.3170188387650512141, 0.3333333333333333703, 0.3170188387650512141, 0.3333333333333333703, 0.3170188387650512141, 0.3333333333333333703, 0.3170188387650512141, 0.3333333333333333703, 0.3170188387650512141, 0.3333333333333333703, 0.3170188387650512141, 0.3333333333333333703, 0.3170188387650512141, 0.3333333333333333703, 0.3170188387650512141, 0.3333333333333333703, 0.3170188387650512141, 0.3333333333333333703, 0.3170188387650512141, 0.3333333333333333703, 0.3170188387650512141, 0.3333333333333333703, 0.3170188387650512141, 0.3333333333333333703, 0.3170188387650512141, 0.3333333333333333703, 0.3170188387650512141, 0.3333333333333333703, 0.3170188387650512141, 0.3333333333333333703, 0.3170188387650512141, 0.3333333333333333703, 0.3170188387650512141, 0.3333333333333333703, 0.3170188387650512141, 0.3333333333333333703, 0.3170188387650512141, 0.3333333333333333703, 0.3170188387650512141, 0.3333333333333333703, 0.3170188387650512141, 0.3333333333333333703, 0.3170188387650512141, 0.3333333333333333703, 0.3170188387650512141, 0.3333333333333333703, 0.3170188387650512141, 0.3333333333333333703, 0.3170188387650512141, 0.3333333333333333703, 0.3170188387650512141, 0.3333333333333333703, 0.3170188387650512141, 0.3333333333333333703, 0.3170188387650512141, 0.3333333333333333703, 0.3170188387650512141, 0.3333333333333333703, 0.3170188387650512141, 0.3333333333333333703, 0.3170188387650512141, 0.3333333333333333703, 0.3170188387650512141, 0.3333333333333333703, 0.3170188387650512141, 0.3333333333333333703, 0.3170188387650512141, 0.3333333333333333703, 0.3170188387650512141, 0.3333333333333333703, 0.3170188387650512141, 0.3333333333333333703, 0.3170188387650512141, 0.3333333333333333703, 0.3170188387650512141, 0.3333333333333333703, 0.3170188387650512141, 0.3333333333333333703, 0.3170188387650512141, 0.3333333333333333703, 0.3170188387650512141, 0.3333333333333333703, 0.3170188387650512141, 0.3333333333333333703, 0.3170188387650512141, 0.3333333333333333703, 0.3170188387650512141, 0.3333333333333333703, 0.3170188387650512141, 0.3333333333333333703, 0.3170188387650512141, 0.3333333333333333703, 0.3170188387650512141, 0.3333333333333333703, 0.3170188387650512141, 0.3333333333333333703, 0.3170188387650512141, 0.3333333333333333703, 0.3170188387650512141, 0.3333333333333333703, 0.3170188387650512141, 0.3333333333333333703, 0.3170188387650512141, 0.3333333333333333703, 0.3170188387650512141, 0.3333333333333333703, 0.3170188387650512141, 0.3333333333333333703, 0.3170188387650512141, 0.3333333333333333703, 0.3170188387650512141, 0.3333333333333333703, 0.3170188387650512141, 0.3333333333333333703, 0.3170188387650512141, 0.3333333333333333703, 0.3170188387650512141, 0.3333333333333333703, 0.3170188387650512141, 0.3333333333333333703, 0.3170188387650512141, 0.3333333333333333703, 0.3170188387650512141, 0.3333333333333333703, 0.3170188387650512141, 0.3333333333333333703, 0.3170188387650512141, 0.3333333333333333703, 0.3170188387650512141, 0.3333333333333333703, 0.3170188387650512141, 0.3333333333333333703, 0.3170188387650512141, 0.3333333333333333703, 0.3170188387650512141, 0.3333333333333333703, 0.3170188387650512141, 0.3333333333333333703, 0.3170188387650512141, 0.3333333333333333703, 0.3170188387650512141, 0.3333333333333333703, 0.3170188387650512141, 0.3333333333333333703, 0.3170188387650512141, 0.3333333333333333703, 0.3170188387650512141, 0.3333333333333333703, 0.3170188387650512141, 0.3333333333333333703, 0.3170188387650512141, 0.3333333333333333703),
 ( 0.3333333333333333703, 0.3170188387650512141, 0.3333333333333333703, 0.3170188387650512141, 0.3333333333333333703, 0.3170188387650512141, 0.3333333333333333703, 0.3170188387650512141, 0.3333333333333333703, 0.3170188387650512141, 0.3333333333333333703, 0.3170188387650512141, 0.3333333333333333703, 0.3170188387650512141, 0.3333333333333333703, 0.3170188387650512141, 0.3333333333333333703, 0.3170188387650512141, 0.3333333333333333703, 0.3170188387650512141, 0.3333333333333333703, 0.3170188387650512141, 0.3333333333333333703, 0.3170188387650512141, 0.3333333333333333703, 0.3170188387650512141, 0.3333333333333333703, 0.3170188387650512141, 0.3333333333333333703, 0.3170188387650512141, 0.3333333333333333703, 0.3170188387650512141, 0.3333333333333333703, 0.3170188387650512141, 0.3333333333333333703, 0.3170188387650512141, 0.3333333333333333703, 0.3170188387650512141, 0.3333333333333333703, 0.3170188387650512141, 0.3333333333333333703, 0.3170188387650512141, 0.3333333333333333703, 0.3170188387650512141, 0.3333333333333333703, 0.3170188387650512141, 0.3333333333333333703, 0.3170188387650512141, 0.3333333333333333703, 0.3170188387650512141, 0.3333333333333333703, 0.3170188387650512141, 0.3333333333333333703, 0.3170188387650512141, 0.3333333333333333703, 0.3170188387650512141, 0.3333333333333333703, 0.3170188387650512141, 0.3333333333333333703, 0.3170188387650512141, 0.3333333333333333703, 0.3170188387650512141, 0.3333333333333333703, 0.3170188387650512141, 0.3333333333333333703, 0.3170188387650512141, 0.3333333333333333703, 0.3170188387650512141, 0.3333333333333333703, 0.3170188387650512141, 0.3333333333333333703, 0.3170188387650512141, 0.3333333333333333703, 0.3170188387650512141, 0.3333333333333333703, 0.3170188387650512141, 0.3333333333333333703, 0.3170188387650512141, 0.3333333333333333703, 0.3170188387650512141, 0.3333333333333333703, 0.3170188387650512141, 0.3333333333333333703, 0.3170188387650512141, 0.3333333333333333703, 0.3170188387650512141, 0.3333333333333333703, 0.3170188387650512141, 0.3333333333333333703, 0.3170188387650512141, 0.3333333333333333703, 0.3170188387650512141, 0.3333333333333333703, 0.3170188387650512141, 0.3333333333333333703, 0.3170188387650512141, 0.3333333333333333703, 0.3170188387650512141, 0.3333333333333333703, 0.3170188387650512141, 0.3333333333333333703, 0.3170188387650512141, 0.3333333333333333703, 0.3170188387650512141, 0.3333333333333333703, 0.3170188387650512141, 0.3333333333333333703, 0.3170188387650512141, 0.3333333333333333703, 0.3170188387650512141, 0.3333333333333333703, 0.3170188387650512141, 0.3333333333333333703, 0.3170188387650512141, 0.3333333333333333703, 0.3170188387650512141, 0.3333333333333333703, 0.3170188387650512141, 0.3333333333333333703, 0.3170188387650512141, 0.3333333333333333703, 0.3170188387650512141, 0.3333333333333333703, 0.3170188387650512141, 0.3333333333333333703, 0.3170188387650512141, 0.3333333333333333703, 0.3170188387650512141, 0.3333333333333333703, 0.3170188387650512141, 0.3333333333333333703, 0.3170188387650512141, 0.3333333333333333703, 0.3170188387650512141, 0.3333333333333333703, 0.3170188387650512141, 0.3333333333333333703, 0.3170188387650512141, 0.3333333333333333703, 0.3170188387650512141, 0.3333333333333333703, 0.3170188387650512141, 0.3333333333333333703, 0.3170188387650512141, 0.3333333333333333703, 0.3170188387650512141, 0.3333333333333333703, 0.3170188387650512141, 0.3333333333333333703, 0.3170188387650512141, 0.3333333333333333703, 0.3170188387650512141, 0.3333333333333333703, 0.3170188387650512141, 0.3333333333333333703, 0.3170188387650512141, 0.3333333333333333703, 0.3170188387650512141, 0.3333333333333333703, 0.3170188387650512141, 0.3333333333333333703, 0.3170188387650512141, 0.3333333333333333703, 0.3170188387650512141, 0.3333333333333333703, 0.3170188387650512141, 0.3333333333333333703, 0.3170188387650512141, 0.3333333333333333703, 0.3170188387650512141, 0.3333333333333333703, 0.3170188387650512141, 0.3333333333333333703, 0.3170188387650512141, 0.3333333333333333703, 0.3170188387650512141, 0.3333333333333333703, 0.3170188387650512141, 0.3333333333333333703, 0.3170188387650512141, 0.3333333333333333703, 0.3170188387650512141, 0.3333333333333333703, 0.3170188387650512141, 0.3333333333333333703, 0.3170188387650512141, 0.3333333333333333703, 0.3170188387650512141, 0.3333333333333333703, 0.3170188387650512141, 0.3333333333333333703, 0.3170188387650512141, 0.3333333333333333703, 0.3170188387650512141, 0.3333333333333333703, 0.3170188387650512141, 0.3333333333333333703, 0.3170188387650512141, 0.3333333333333333703, 0.3170188387650512141, 0.3333333333333333703),
 ( 1.000000000000000000, 0.9510565162951535312, 1.000000000000000000, 0.9510565162951535312, 1.000000000000000000, 0.9510565162951535312, 1.000000000000000000, 0.9510565162951535312, 1.000000000000000000, 0.9510565162951535312, 1.000000000000000000, 0.9510565162951535312, 1.000000000000000000, 0.9510565162951535312, 1.000000000000000000, 0.9510565162951535312, 1.000000000000000000, 0.9510565162951535312, 1.000000000000000000, 0.9510565162951535312, 1.000000000000000000, 0.9510565162951535312, 1.000000000000000000, 0.9510565162951535312, 1.000000000000000000, 0.9510565162951535312, 1.000000000000000000, 0.9510565162951535312, 1.000000000000000000, 0.9510565162951535312, 1.000000000000000000, 0.9510565162951535312, 1.000000000000000000, 0.9510565162951535312, 1.000000000000000000, 0.9510565162951535312, 1.000000000000000000, 0.9510565162951535312, 1.000000000000000000, 0.9510565162951535312, 1.000000000000000000, 0.9510565162951535312, 1.000000000000000000, 0.9510565162951535312, 1.000000000000000000, 0.9510565162951535312, 1.000000000000000000, 0.9510565162951535312, 1.000000000000000000, 0.9510565162951535312, 1.000000000000000000, 0.9510565162951535312, 1.000000000000000000, 0.9510565162951535312, 1.000000000000000000, 0.9510565162951535312, 1.000000000000000000, 0.9510565162951535312, 1.000000000000000000, 0.9510565162951535312, 1.000000000000000000, 0.9510565162951535312, 1.000000000000000000, 0.9510565162951535312, 1.000000000000000000, 0.9510565162951535312, 1.000000000000000000, 0.9510565162951535312, 1.000000000000000000, 0.9510565162951535312, 1.000000000000000000, 0.9510565162951535312, 1.000000000000000000, 0.9510565162951535312, 1.000000000000000000, 0.9510565162951535312, 1.000000000000000000, 0.9510565162951535312, 1.000000000000000000, 0.9510565162951535312, 1.000000000000000000, 0.9510565162951535312, 1.000000000000000000, 0.9510565162951535312, 1.000000000000000000, 0.9510565162951535312, 1.000000000000000000, 0.9510565162951535312, 1.000000000000000000, 0.9510565162951535312, 1.000000000000000000, 0.9510565162951535312, 1.000000000000000000, 0.9510565162951535312, 1.000000000000000000, 0.9510565162951535312, 1.000000000000000000, 0.9510565162951535312, 1.000000000000000000, 0.9510565162951535312, 1.000000000000000000, 0.9510565162951535312, 1.000000000000000000, 0.9510565162951535312, 1.000000000000000000, 0.9510565162951535312, 1.000000000000000000, 0.9510565162951535312, 1.000000000000000000, 0.9510565162951535312, 1.000000000000000000, 0.9510565162951535312, 1.000000000000000000, 0.9510565162951535312, 1.000000000000000000, 0.9510565162951535312, 1.000000000000000000, 0.9510565162951535312, 1.000000000000000000, 0.9510565162951535312, 1.000000000000000000, 0.9510565162951535312, 1.000000000000000000, 0.9510565162951535312, 1.000000000000000000, 0.9510565162951535312, 1.000000000000000000, 0.9510565162951535312, 1.000000000000000000, 0.9510565162951535312, 1.000000000000000000, 0.9510565162951535312, 1.000000000000000000, 0.9510565162951535312, 1.000000000000000000, 0.9510565162951535312, 1.000000000000000000, 0.9510565162951535312, 1.000000000000000000, 0.9510565162951535312, 1.000000000000000000, 0.9510565162951535312, 1.000000000000000000, 0.9510565162951535312, 1.000000000000000000, 0.9510565162951535312, 1.000000000000000000, 0.9510565162951535312, 1.000000000000000000, 0.9510565162951535312, 1.000000000000000000, 0.9510565162951535312, 1.000000000000000000, 0.9510565162951535312, 1.000000000000000000, 0.9510565162951535312, 1.000000000000000000, 0.9510565162951535312, 1.000000000000000000, 0.9510565162951535312, 1.000000000000000000, 0.9510565162951535312, 1.000000000000000000, 0.9510565162951535312, 1.000000000000000000, 0.9510565162951535312, 1.000000000000000000, 0.9510565162951535312, 1.000000000000000000, 0.9510565162951535312, 1.000000000000000000, 0.9510565162951535312, 1.000000000000000000, 0.9510565162951535312, 1.000000000000000000, 0.9510565162951535312, 1.000000000000000000, 0.9510565162951535312, 1.000000000000000000, 0.9510565162951535312, 1.000000000000000000, 0.9510565162951535312, 1.000000000000000000, 0.9510565162951535312, 1.000000000000000000, 0.9510565162951535312, 1.000000000000000000, 0.9510565162951535312, 1.000000000000000000, 0.9510565162951535312, 1.000000000000000000, 0.9510565162951535312, 1.000000000000000000, 0.9510565162951535312, 1.000000000000000000, 0.9510565162951535312, 1.000000000000000000, 0.9510565162951535312, 1.000000000000000000, 0.9510565162951535312, 1.000000000000000000),
 ( 0.3333333333333333703, 0.3170188387650512141, 0.3333333333333333703, 0.3170188387650512141, 0.3333333333333333703, 0.3170188387650512141, 0.3333333333333333703, 0.3170188387650512141, 0.3333333333333333703, 0.3170188387650512141, 0.3333333333333333703, 0.3170188387650512141, 0.3333333333333333703, 0.3170188387650512141, 0.3333333333333333703, 0.3170188387650512141, 0.3333333333333333703, 0.3170188387650512141, 0.3333333333333333703, 0.3170188387650512141, 0.3333333333333333703, 0.3170188387650512141, 0.3333333333333333703, 0.3170188387650512141, 0.3333333333333333703, 0.3170188387650512141, 0.3333333333333333703, 0.3170188387650512141, 0.3333333333333333703, 0.3170188387650512141, 0.3333333333333333703, 0.3170188387650512141, 0.3333333333333333703, 0.3170188387650512141, 0.3333333333333333703, 0.3170188387650512141, 0.3333333333333333703, 0.3170188387650512141, 0.3333333333333333703, 0.3170188387650512141, 0.3333333333333333703, 0.3170188387650512141, 0.3333333333333333703, 0.3170188387650512141, 0.3333333333333333703, 0.3170188387650512141, 0.3333333333333333703, 0.3170188387650512141, 0.3333333333333333703, 0.3170188387650512141, 0.3333333333333333703, 0.3170188387650512141, 0.3333333333333333703, 0.3170188387650512141, 0.3333333333333333703, 0.3170188387650512141, 0.3333333333333333703, 0.3170188387650512141, 0.3333333333333333703, 0.3170188387650512141, 0.3333333333333333703, 0.3170188387650512141, 0.3333333333333333703, 0.3170188387650512141, 0.3333333333333333703, 0.3170188387650512141, 0.3333333333333333703, 0.3170188387650512141, 0.3333333333333333703, 0.3170188387650512141, 0.3333333333333333703, 0.3170188387650512141, 0.3333333333333333703, 0.3170188387650512141, 0.3333333333333333703, 0.3170188387650512141, 0.3333333333333333703, 0.3170188387650512141, 0.3333333333333333703, 0.3170188387650512141, 0.3333333333333333703, 0.3170188387650512141, 0.3333333333333333703, 0.3170188387650512141, 0.3333333333333333703, 0.3170188387650512141, 0.3333333333333333703, 0.3170188387650512141, 0.3333333333333333703, 0.3170188387650512141, 0.3333333333333333703, 0.3170188387650512141, 0.3333333333333333703, 0.3170188387650512141, 0.3333333333333333703, 0.3170188387650512141, 0.3333333333333333703, 0.3170188387650512141, 0.3333333333333333703, 0.3170188387650512141, 0.3333333333333333703, 0.3170188387650512141, 0.3333333333333333703, 0.3170188387650512141, 0.3333333333333333703, 0.3170188387650512141, 0.3333333333333333703, 0.3170188387650512141, 0.3333333333333333703, 0.3170188387650512141, 0.3333333333333333703, 0.3170188387650512141, 0.3333333333333333703, 0.3170188387650512141, 0.3333333333333333703, 0.3170188387650512141, 0.3333333333333333703, 0.3170188387650512141, 0.3333333333333333703, 0.3170188387650512141, 0.3333333333333333703, 0.3170188387650512141, 0.3333333333333333703, 0.3170188387650512141, 0.3333333333333333703, 0.3170188387650512141, 0.3333333333333333703, 0.3170188387650512141, 0.3333333333333333703, 0.3170188387650512141, 0.3333333333333333703, 0.3170188387650512141, 0.3333333333333333703, 0.3170188387650512141, 0.3333333333333333703, 0.3170188387650512141, 0.3333333333333333703, 0.3170188387650512141, 0.3333333333333333703, 0.3170188387650512141, 0.3333333333333333703, 0.3170188387650512141, 0.3333333333333333703, 0.3170188387650512141, 0.3333333333333333703, 0.3170188387650512141, 0.3333333333333333703, 0.3170188387650512141, 0.3333333333333333703, 0.3170188387650512141, 0.3333333333333333703, 0.3170188387650512141, 0.3333333333333333703, 0.3170188387650512141, 0.3333333333333333703, 0.3170188387650512141, 0.3333333333333333703, 0.3170188387650512141, 0.3333333333333333703, 0.3170188387650512141, 0.3333333333333333703, 0.3170188387650512141, 0.3333333333333333703, 0.3170188387650512141, 0.3333333333333333703, 0.3170188387650512141, 0.3333333333333333703, 0.3170188387650512141, 0.3333333333333333703, 0.3170188387650512141, 0.3333333333333333703, 0.3170188387650512141, 0.3333333333333333703, 0.3170188387650512141, 0.3333333333333333703, 0.3170188387650512141, 0.3333333333333333703, 0.3170188387650512141, 0.3333333333333333703, 0.3170188387650512141, 0.3333333333333333703, 0.3170188387650512141, 0.3333333333333333703, 0.3170188387650512141, 0.3333333333333333703, 0.3170188387650512141, 0.3333333333333333703, 0.3170188387650512141, 0.3333333333333333703, 0.3170188387650512141, 0.3333333333333333703, 0.3170188387650512141, 0.3333333333333333703, 0.3170188387650512141, 0.3333333333333333703, 0.3170188387650512141, 0.3333333333333333703, 0.3170188387650512141, 0.3333333333333333703, 0.3170188387650512141, 0.3333333333333333703),
 ( 0.3333333333333333703, 0.3170188387650512141, 0.3333333333333333703, 0.3170188387650512141, 0.3333333333333333703, 0.3170188387650512141, 0.3333333333333333703, 0.3170188387650512141, 0.3333333333333333703, 0.3170188387650512141, 0.3333333333333333703, 0.3170188387650512141, 0.3333333333333333703, 0.3170188387650512141, 0.3333333333333333703, 0.3170188387650512141, 0.3333333333333333703, 0.3170188387650512141, 0.3333333333333333703, 0.3170188387650512141, 0.3333333333333333703, 0.3170188387650512141, 0.3333333333333333703, 0.3170188387650512141, 0.3333333333333333703, 0.3170188387650512141, 0.3333333333333333703, 0.3170188387650512141, 0.3333333333333333703, 0.3170188387650512141, 0.3333333333333333703, 0.3170188387650512141, 0.3333333333333333703, 0.3170188387650512141, 0.3333333333333333703, 0.3170188387650512141, 0.3333333333333333703, 0.3170188387650512141, 0.3333333333333333703, 0.3170188387650512141, 0.3333333333333333703, 0.3170188387650512141, 0.3333333333333333703, 0.3170188387650512141, 0.3333333333333333703, 0.3170188387650512141, 0.3333333333333333703, 0.3170188387650512141, 0.3333333333333333703, 0.3170188387650512141, 0.3333333333333333703, 0.3170188387650512141, 0.3333333333333333703, 0.3170188387650512141, 0.3333333333333333703, 0.3170188387650512141, 0.3333333333333333703, 0.3170188387650512141, 0.3333333333333333703, 0.3170188387650512141, 0.3333333333333333703, 0.3170188387650512141, 0.3333333333333333703, 0.3170188387650512141, 0.3333333333333333703, 0.3170188387650512141, 0.3333333333333333703, 0.3170188387650512141, 0.3333333333333333703, 0.3170188387650512141, 0.3333333333333333703, 0.3170188387650512141, 0.3333333333333333703, 0.3170188387650512141, 0.3333333333333333703, 0.3170188387650512141, 0.3333333333333333703, 0.3170188387650512141, 0.3333333333333333703, 0.3170188387650512141, 0.3333333333333333703, 0.3170188387650512141, 0.3333333333333333703, 0.3170188387650512141, 0.3333333333333333703, 0.3170188387650512141, 0.3333333333333333703, 0.3170188387650512141, 0.3333333333333333703, 0.3170188387650512141, 0.3333333333333333703, 0.3170188387650512141, 0.3333333333333333703, 0.3170188387650512141, 0.3333333333333333703, 0.3170188387650512141, 0.3333333333333333703, 0.3170188387650512141, 0.3333333333333333703, 0.3170188387650512141, 0.3333333333333333703, 0.3170188387650512141, 0.3333333333333333703, 0.3170188387650512141, 0.3333333333333333703, 0.3170188387650512141, 0.3333333333333333703, 0.3170188387650512141, 0.3333333333333333703, 0.3170188387650512141, 0.3333333333333333703, 0.3170188387650512141, 0.3333333333333333703, 0.3170188387650512141, 0.3333333333333333703, 0.3170188387650512141, 0.3333333333333333703, 0.3170188387650512141, 0.3333333333333333703, 0.3170188387650512141, 0.3333333333333333703, 0.3170188387650512141, 0.3333333333333333703, 0.3170188387650512141, 0.3333333333333333703, 0.3170188387650512141, 0.3333333333333333703, 0.3170188387650512141, 0.3333333333333333703, 0.3170188387650512141, 0.3333333333333333703, 0.3170188387650512141, 0.3333333333333333703, 0.3170188387650512141, 0.3333333333333333703, 0.3170188387650512141, 0.3333333333333333703, 0.3170188387650512141, 0.3333333333333333703, 0.3170188387650512141, 0.3333333333333333703, 0.3170188387650512141, 0.3333333333333333703, 0.3170188387650512141, 0.3333333333333333703, 0.3170188387650512141, 0.3333333333333333703, 0.3170188387650512141, 0.3333333333333333703, 0.3170188387650512141, 0.3333333333333333703, 0.3170188387650512141, 0.3333333333333333703, 0.3170188387650512141, 0.3333333333333333703, 0.3170188387650512141, 0.3333333333333333703, 0.3170188387650512141, 0.3333333333333333703, 0.3170188387650512141, 0.3333333333333333703, 0.3170188387650512141, 0.3333333333333333703, 0.3170188387650512141, 0.3333333333333333703, 0.3170188387650512141, 0.3333333333333333703, 0.3170188387650512141, 0.3333333333333333703, 0.3170188387650512141, 0.3333333333333333703, 0.3170188387650512141, 0.3333333333333333703, 0.3170188387650512141, 0.3333333333333333703, 0.3170188387650512141, 0.3333333333333333703, 0.3170188387650512141, 0.3333333333333333703, 0.3170188387650512141, 0.3333333333333333703, 0.3170188387650512141, 0.3333333333333333703, 0.3170188387650512141, 0.3333333333333333703, 0.3170188387650512141, 0.3333333333333333703, 0.3170188387650512141, 0.3333333333333333703, 0.3170188387650512141, 0.3333333333333333703, 0.3170188387650512141, 0.3333333333333333703, 0.3170188387650512141, 0.3333333333333333703, 0.3170188387650512141, 0.3333333333333333703, 0.3170188387650512141, 0.3333333333333333703, 0.3170188387650512141, 0.3333333333333333703),
 ( 1.000000000000000000, 0.9510565162951535312, 1.000000000000000000, 0.9510565162951535312, 1.000000000000000000, 0.9510565162951535312, 1.000000000000000000, 0.9510565162951535312, 1.000000000000000000, 0.9510565162951535312, 1.000000000000000000, 0.9510565162951535312, 1.000000000000000000, 0.9510565162951535312, 1.000000000000000000, 0.9510565162951535312, 1.000000000000000000, 0.9510565162951535312, 1.000000000000000000, 0.9510565162951535312, 1.000000000000000000, 0.9510565162951535312, 1.000000000000000000, 0.9510565162951535312, 1.000000000000000000, 0.9510565162951535312, 1.000000000000000000, 0.9510565162951535312, 1.000000000000000000, 0.9510565162951535312, 1.000000000000000000, 0.9510565162951535312, 1.000000000000000000, 0.9510565162951535312, 1.000000000000000000, 0.9510565162951535312, 1.000000000000000000, 0.9510565162951535312, 1.000000000000000000, 0.9510565162951535312, 1.000000000000000000, 0.9510565162951535312, 1.000000000000000000, 0.9510565162951535312, 1.000000000000000000, 0.9510565162951535312, 1.000000000000000000, 0.9510565162951535312, 1.000000000000000000, 0.9510565162951535312, 1.000000000000000000, 0.9510565162951535312, 1.000000000000000000, 0.9510565162951535312, 1.000000000000000000, 0.9510565162951535312, 1.000000000000000000, 0.9510565162951535312, 1.000000000000000000, 0.9510565162951535312, 1.000000000000000000, 0.9510565162951535312, 1.000000000000000000, 0.9510565162951535312, 1.000000000000000000, 0.9510565162951535312, 1.000000000000000000, 0.9510565162951535312, 1.000000000000000000, 0.9510565162951535312, 1.000000000000000000, 0.9510565162951535312, 1.000000000000000000, 0.9510565162951535312, 1.000000000000000000, 0.9510565162951535312, 1.000000000000000000, 0.9510565162951535312, 1.000000000000000000, 0.9510565162951535312, 1.000000000000000000, 0.9510565162951535312, 1.000000000000000000, 0.9510565162951535312, 1.000000000000000000, 0.9510565162951535312, 1.000000000000000000, 0.9510565162951535312, 1.000000000000000000, 0.9510565162951535312, 1.000000000000000000, 0.9510565162951535312, 1.000000000000000000, 0.9510565162951535312, 1.000000000000000000, 0.9510565162951535312, 1.000000000000000000, 0.9510565162951535312, 1.000000000000000000, 0.9510565162951535312, 1.000000000000000000, 0.9510565162951535312, 1.000000000000000000, 0.9510565162951535312, 1.000000000000000000, 0.9510565162951535312, 1.000000000000000000, 0.9510565162951535312, 1.000000000000000000, 0.9510565162951535312, 1.000000000000000000, 0.9510565162951535312, 1.000000000000000000, 0.9510565162951535312, 1.000000000000000000, 0.9510565162951535312, 1.000000000000000000, 0.9510565162951535312, 1.000000000000000000, 0.9510565162951535312, 1.000000000000000000, 0.9510565162951535312, 1.000000000000000000, 0.9510565162951535312, 1.000000000000000000, 0.9510565162951535312, 1.000000000000000000, 0.9510565162951535312, 1.000000000000000000, 0.9510565162951535312, 1.000000000000000000, 0.9510565162951535312, 1.000000000000000000, 0.9510565162951535312, 1.000000000000000000, 0.9510565162951535312, 1.000000000000000000, 0.9510565162951535312, 1.000000000000000000, 0.9510565162951535312, 1.000000000000000000, 0.9510565162951535312, 1.000000000000000000, 0.9510565162951535312, 1.000000000000000000, 0.9510565162951535312, 1.000000000000000000, 0.9510565162951535312, 1.000000000000000000, 0.9510565162951535312, 1.000000000000000000, 0.9510565162951535312, 1.000000000000000000, 0.9510565162951535312, 1.000000000000000000, 0.9510565162951535312, 1.000000000000000000, 0.9510565162951535312, 1.000000000000000000, 0.9510565162951535312, 1.000000000000000000, 0.9510565162951535312, 1.000000000000000000, 0.9510565162951535312, 1.000000000000000000, 0.9510565162951535312, 1.000000000000000000, 0.9510565162951535312, 1.000000000000000000, 0.9510565162951535312, 1.000000000000000000, 0.9510565162951535312, 1.000000000000000000, 0.9510565162951535312, 1.000000000000000000, 0.9510565162951535312, 1.000000000000000000, 0.9510565162951535312, 1.000000000000000000, 0.9510565162951535312, 1.000000000000000000, 0.9510565162951535312, 1.000000000000000000, 0.9510565162951535312, 1.000000000000000000, 0.9510565162951535312, 1.000000000000000000, 0.9510565162951535312, 1.000000000000000000, 0.9510565162951535312, 1.000000000000000000, 0.9510565162951535312, 1.000000000000000000, 0.9510565162951535312, 1.000000000000000000, 0.9510565162951535312, 1.000000000000000000, 0.9510565162951535312, 1.000000000000000000, 0.9510565162951535312, 1.000000000000000000) ) ) 
 REPRESENTATION_ITEM ( '' )  SURFACE ( )  );
#12726 = EDGE_CURVE ( 'NONE', #2412, #18202, #14434, .T. ) ;
#12727 = CARTESIAN_POINT ( 'NONE',  ( -2.121784821874996396, -19.64232189773168358, -10.17789796607362618 ) ) ;
#12728 = EDGE_CURVE ( 'NONE', #14997, #13741, #4995, .T. ) ;
#12729 = DIRECTION ( 'NONE',  ( -0.000000000000000000, 1.000000000000000000, -0.000000000000000000 ) ) ;
#12730 = CIRCLE ( 'NONE', #6212, 2.499999999999999556 ) ;
#12731 = CARTESIAN_POINT ( 'NONE',  ( -13.00000000000000178, 15.00000000000000178, 16.00000000000000000 ) ) ;
#12732 = AXIS2_PLACEMENT_3D ( 'NONE', #5900, #4328, #71 ) ;
#12733 = DIRECTION ( 'NONE',  ( -0.000000000000000000, 1.000000000000000000, -0.000000000000000000 ) ) ;
#12734 = CARTESIAN_POINT ( 'NONE',  ( 2.121784821874994176, -24.21128814972218990, -3.888587676801722903 ) ) ;
#12735 = CARTESIAN_POINT ( 'NONE',  ( -1.127657100080120323, 15.00000000000000888, -3.191926594068459799 ) ) ;
#12736 = DIRECTION ( 'NONE',  ( 0.000000000000000000, 0.8191520442889950182, -0.5735764363510414965 ) ) ;
#12737 = ORIENTED_EDGE ( 'NONE', *, *, #8396, .T. ) ;
#12738 = CARTESIAN_POINT ( 'NONE',  ( 2.481649420246391902, 20.87819992234355126, 0.8687765177875720335 ) ) ;
#12739 = CARTESIAN_POINT ( 'NONE',  ( -8.500000000000007105, 14.99364916731036956, -20.49999999999999645 ) ) ;
#12740 = CARTESIAN_POINT ( 'NONE',  ( -3.518350579753630747, 18.12180007765648071, -1.080741659609802729 ) ) ;
#12741 = DIRECTION ( 'NONE',  ( 0.000000000000000000, 0.000000000000000000, -1.000000000000000000 ) ) ;
#12742 = DIRECTION ( 'NONE',  ( -0.000000000000000000, 0.000000000000000000, 1.000000000000000000 ) ) ;
#12743 = EDGE_LOOP ( 'NONE', ( #15644, #3038, #6933, #13168 ) ) ;
#12744 = CARTESIAN_POINT ( 'NONE',  ( 4.243569643749997233, -21.92802379169658877, -2.763493290842798267 ) ) ;
#12745 = AXIS2_PLACEMENT_3D ( 'NONE', #15700, #7154, #212 ) ;
#12746 = CARTESIAN_POINT ( 'NONE',  ( 2.211161402132902243, 32.12180007765647360, 2.942372952327172442 ) ) ;
#12747 = DIRECTION ( 'NONE',  ( 0.000000000000000000, 0.000000000000000000, -1.000000000000000000 ) ) ;
#12748 = CARTESIAN_POINT ( 'NONE',  ( -2.121784821875005722, -29.15838491324991466, -10.95377405879430910 ) ) ;
#12749 = CARTESIAN_POINT ( 'NONE',  ( 2.021687836487040535, 2.168404344971008868E-16, 0.000000000000000000 ) ) ;
#12750 = LINE ( 'NONE', #5343, #6199 ) ;
#12751 = LINE ( 'NONE', #11435, #2314 ) ;
#12752 = CARTESIAN_POINT ( 'NONE',  ( 4.243569643750003451, -22.74293267755752623, -12.47028401514436169 ) ) ;
#12753 = ORIENTED_EDGE ( 'NONE', *, *, #8583, .T. ) ;
#12754 = CARTESIAN_POINT ( 'NONE',  ( -1.661723472263481630E-14, -20.51073541163217584, -11.98467301000088803 ) ) ;
#12755 = CARTESIAN_POINT ( 'NONE',  ( 1.999999999999994449, -23.69972968376769273, -3.525764780161007472 ) ) ;
#12756 = AXIS2_PLACEMENT_3D ( 'NONE', #1279, #12390, #15549 ) ;
#12757 = CARTESIAN_POINT ( 'NONE',  ( 0.7188294034286049072, 23.74680007765648426, -2.395093729190366005 ) ) ;
#12758 = EDGE_LOOP ( 'NONE', ( #3376, #858, #455, #595 ) ) ;
#12759 = CARTESIAN_POINT ( 'NONE',  ( 3.083285004801276763, -24.87914370749852822, -15.73138478113422778 ) ) ;
#12760 = DIRECTION ( 'NONE',  ( -3.469446951953613696E-16, -0.000000000000000000, -1.000000000000000000 ) ) ;
#12761 = CARTESIAN_POINT ( 'NONE',  ( -1.989345975306457071, 37.25319992234354061, -1.515154207786300944 ) ) ;
#12762 = EDGE_LOOP ( 'NONE', ( #7008, #12508, #13770, #18337 ) ) ;
#12763 = CARTESIAN_POINT ( 'NONE',  ( 2.121784821874994176, -26.82464578784662379, -7.620849178593458007 ) ) ;
#12764 = CARTESIAN_POINT ( 'NONE',  ( 2.733110507866247652, 31.37180007765647716, -3.862833514489153686 ) ) ;
#12765 = ORIENTED_EDGE ( 'NONE', *, *, #9170, .F. ) ;
#12766 = VECTOR ( 'NONE', #4470, 1000.000000000000000 ) ;
#12767 = CARTESIAN_POINT ( 'NONE',  ( 3.999999999999996447, 6.938893903907228378E-15, 0.000000000000000000 ) ) ;
#12768 = CARTESIAN_POINT ( 'NONE',  ( 9.000000000000005329, 38.59999999999999432, 2.499999999999997335 ) ) ;
#12769 = SHAPE_REPRESENTATION ( 'seal', ( #16940 ), #340 ) ;
#12770 = CARTESIAN_POINT ( 'NONE',  ( 8.500000000000019540, 0.000000000000000000, 20.49999999999998934 ) ) ;
#12771 = LINE ( 'NONE', #16881, #9163 ) ;
#12772 = CARTESIAN_POINT ( 'NONE',  ( -1.999999999999996225, -23.25119311998180649, -14.96414190187491400 ) ) ;
#12773 = CARTESIAN_POINT ( 'NONE',  ( -2.121784821875005722, -24.54467945335122536, -4.364719802544705374 ) ) ;
#12774 = VERTEX_POINT ( 'NONE', #2626 ) ;
#12775 = ORIENTED_EDGE ( 'NONE', *, *, #15610, .F. ) ;
#12776 = EDGE_LOOP ( 'NONE', ( #1734, #16796, #10074, #10372 ) ) ;
#12777 = FACE_OUTER_BOUND ( 'NONE', #7488, .T. ) ;
#12778 = CARTESIAN_POINT ( 'NONE',  ( -3.607379964056363075, 17.25319992234354416, -2.690724712371229899 ) ) ;
#12779 = CARTESIAN_POINT ( 'NONE',  ( 0.05938372350920110426, 25.12819992234354416, -3.680117784833935701 ) ) ;
#12780 = EDGE_CURVE ( 'NONE', #12103, #159, #18227, .T. ) ;
#12781 = CARTESIAN_POINT ( 'NONE',  ( -4.000000000000004441, -27.72246025710361295, -11.28397838367063244 ) ) ;
#12782 = CARTESIAN_POINT ( 'NONE',  ( -0.7188294034286043521, 34.99680007765648071, 2.395093729190366005 ) ) ;
#12783 = CIRCLE ( 'NONE', #4797, 7.000000000000000000 ) ;
#12784 = CARTESIAN_POINT ( 'NONE',  ( 1.336863392178569754, 36.25319992234354771, 4.297206761780648421 ) ) ;
#12785 = CARTESIAN_POINT ( 'NONE',  ( -3.999999999999997335, -22.11068413930986054, -11.32216732091749556 ) ) ;
#12786 = VERTEX_POINT ( 'NONE', #17462 ) ;
#12787 = CIRCLE ( 'NONE', #13081, 1.899999999999999689 ) ;
#12788 = CARTESIAN_POINT ( 'NONE',  ( -8.500000000000005329, 10.00000000000000000, 22.50000000000000000 ) ) ;
#12789 = COLOUR_RGB ( '',0.8941176470588234615, 0.8941176470588234615, 0.8941176470588234615 ) ;
#12790 = CARTESIAN_POINT ( 'NONE',  ( 2.211161402132902243, 24.62180007765647716, 2.942372952327172442 ) ) ;
#12791 = CARTESIAN_POINT ( 'NONE',  ( -7.316869269719566304, -13.46470072737469081, 2.124349773241079653 ) ) ;
#12792 = PRODUCT_DEFINITION_FORMATION_WITH_SPECIFIED_SOURCE ( 'ANY', '', #9448, .NOT_KNOWN. ) ;
#12793 = CARTESIAN_POINT ( 'NONE',  ( -2.121784821874996396, -20.12627701590287543, -10.86905750344246435 ) ) ;
#12794 = CARTESIAN_POINT ( 'NONE',  ( 3.607379964056306676, 26.49680007765647716, -2.690724712371305838 ) ) ;
#12795 = CARTESIAN_POINT ( 'NONE',  ( -1.071796769724496334, -21.59617364613965762, -13.53483946105443003 ) ) ;
#12796 = FACE_OUTER_BOUND ( 'NONE', #1104, .T. ) ;
#12797 = ORIENTED_EDGE ( 'NONE', *, *, #9197, .F. ) ;
#12798 = EDGE_LOOP ( 'NONE', ( #3712, #10743 ) ) ;
#12799 = CARTESIAN_POINT ( 'NONE',  ( -2.211161402132902243, 20.87180007765647716, -2.942372952327172886 ) ) ;
#12800 = CARTESIAN_POINT ( 'NONE',  ( -6.428571428571424384, -11.73421655796351892, 14.25837509840160422 ) ) ;
#12801 = CIRCLE ( 'NONE', #376, 4.000000000000001776 ) ;
#12802 = DIRECTION ( 'NONE',  ( -0.000000000000000000, 1.000000000000000000, -0.000000000000000000 ) ) ;
#12803 = ORIENTED_EDGE ( 'NONE', *, *, #9883, .T. ) ;
#12804 = VECTOR ( 'NONE', #14553, 1000.000000000000000 ) ;
#12805 = CARTESIAN_POINT ( 'NONE',  ( -3.500000000000000444, 22.00319992234354416, -0.05647727720529563400 ) ) ;
#12806 = CARTESIAN_POINT ( 'NONE',  ( -4.243569643750005227, -24.82099994254214437, -6.895091414225420934 ) ) ;
#12807 = CARTESIAN_POINT ( 'NONE',  ( -1.989345975306426206, 17.74680007765647716, 1.515154207786343799 ) ) ;
#12808 = CARTESIAN_POINT ( 'NONE',  ( 1.135272562821020070, 35.25319992234354771, -3.311245368580577164 ) ) ;
#12809 = CARTESIAN_POINT ( 'NONE',  ( -13.00000000000000178, 15.00000000000000178, 16.00000000000000000 ) ) ;
#12810 = PRESENTATION_LAYER_ASSIGNMENT (  '', '', ( #8072 ) ) ;
#12811 = FACE_OUTER_BOUND ( 'NONE', #5956, .T. ) ;
#12812 = CARTESIAN_POINT ( 'NONE',  ( -4.243569643749997233, -20.62428471578586553, -9.444541151551892000 ) ) ;
#12813 = EDGE_CURVE ( 'NONE', #18266, #156, #15649, .T. ) ;
#12814 = AXIS2_PLACEMENT_3D ( 'NONE', #9007, #6224, #2345 ) ;
#12815 = AXIS2_PLACEMENT_3D ( 'NONE', #9836, #15776, #17089 ) ;
#12816 = EDGE_CURVE ( 'NONE', #5386, #935, #17718, .T. ) ;
#12817 = CARTESIAN_POINT ( 'NONE',  ( -6.428571428571426161, -14.26578344203648285, -2.827263138854404279 ) ) ;
#12818 = CARTESIAN_POINT ( 'NONE',  ( -1.734723475976807094E-15, 36.39999999999999147, -11.50000000000000178 ) ) ;
#12819 = LINE ( 'NONE', #4022, #5562 ) ;
#12820 = CARTESIAN_POINT ( 'NONE',  ( -4.243569643750000786, -20.51258062284889760, -5.013521062237622949 ) ) ;
#12821 = CARTESIAN_POINT ( 'NONE',  ( 0.000000000000000000, 5.977523610840987267, 32.81826849749789687 ) ) ;
#12822 = ORIENTED_EDGE ( 'NONE', *, *, #11240, .F. ) ;
#12823 = CARTESIAN_POINT ( 'NONE',  ( 0.7188294034286553114, 21.25319992234354771, 2.395093729190349130 ) ) ;
#12824 = CARTESIAN_POINT ( 'NONE',  ( 4.243569643750003451, -25.06591724477924288, -15.78784979451479309 ) ) ;
#12825 = CARTESIAN_POINT ( 'NONE',  ( -3.518350579753630747, 15.62180007765647538, -1.080741659609802729 ) ) ;
#12826 = AXIS2_PLACEMENT_3D ( 'NONE', #17234, #14155, #8760 ) ;
#12827 = DIRECTION ( 'NONE',  ( -1.000000000000000000, 0.000000000000000000, -0.000000000000000000 ) ) ;
#12828 = CARTESIAN_POINT ( 'NONE',  ( -2.465190328815646976E-33, -26.97786251599082519, -14.24690051095425858 ) ) ;
#12829 = ORIENTED_EDGE ( 'NONE', *, *, #609, .F. ) ;
#12830 = CARTESIAN_POINT ( 'NONE',  ( -4.243569643750004339, -22.53027904986517527, -3.623602937346249941 ) ) ;
#12831 = CARTESIAN_POINT ( 'NONE',  ( -3.518350579753630747, 30.62180007765647716, -1.080741659609802729 ) ) ;
#12832 = CARTESIAN_POINT ( 'NONE',  ( 4.243569643750000786, -26.86852450816387972, -14.09074965301504534 ) ) ;
#12833 = EDGE_CURVE ( 'NONE', #15136, #526, #5757, .T. ) ;
#12834 = EDGE_CURVE ( 'NONE', #7853, #3408, #6117, .T. ) ;
#12835 = CARTESIAN_POINT ( 'NONE',  ( -2.121784821874996396, -22.19115218676662238, -13.81800486288284624 ) ) ;
#12836 = DIRECTION ( 'NONE',  ( -1.000000000000000000, 0.000000000000000000, 4.336808689942021680E-16 ) ) ;
#12837 = TOROIDAL_SURFACE ( 'NONE', #1647, 9.000000000000001776, 0.9999999999999991118 ) ;
#12838 = CARTESIAN_POINT ( 'NONE',  ( -2.000000000000005773, -27.35627946550557255, -8.747859062503353655 ) ) ;
#12839 = CARTESIAN_POINT ( 'NONE',  ( -1.734723475976807094E-15, 27.59999999999999432, -2.500000000000000000 ) ) ;
#12840 = CARTESIAN_POINT ( 'NONE',  ( 2.121784821875004390, -21.97606102313498511, -13.51082284627447017 ) ) ;
#12841 = DIRECTION ( 'NONE',  ( 1.047034504275222322E-14, -0.1129545544106647231, 0.9936001553129348851 ) ) ;
#12842 = CARTESIAN_POINT ( 'NONE',  ( 4.713407268011036227E-15, -16.45483816335116245, -7.271100070990128117 ) ) ;
#12843 = CARTESIAN_POINT ( 'NONE',  ( 2.481649420246374138, 24.12180007765648071, -0.8687765177876252132 ) ) ;
#12844 = ORIENTED_EDGE ( 'NONE', *, *, #3328, .T. ) ;
#12845 = CARTESIAN_POINT ( 'NONE',  ( -3.481649420246370141, 20.37180007765647716, 1.193696214020542268 ) ) ;
#12846 = DIRECTION ( 'NONE',  ( -0.000000000000000000, 1.000000000000000000, -0.000000000000000000 ) ) ;
#12847 = LINE ( 'NONE', #10244, #11950 ) ;
#12848 = CARTESIAN_POINT ( 'NONE',  ( -2.798362969681409851, 14.75319992234354594, -2.102939460078765421 ) ) ;
#12849 = VERTEX_POINT ( 'NONE', #4633 ) ;
#12850 = CARTESIAN_POINT ( 'NONE',  ( -4.243569643749998122, -22.43105049029164277, -12.02487009106222615 ) ) ;
#12851 = CARTESIAN_POINT ( 'NONE',  ( 3.673772985318219053, 34.49680007765647360, 2.599342558260951730 ) ) ;
#12852 = ADVANCED_FACE ( 'NONE', ( #1781, #6024 ), #17273, .F. ) ;
#12853 = ORIENTED_EDGE ( 'NONE', *, *, #1503, .T. ) ;
#12854 = DIRECTION ( 'NONE',  ( 0.000000000000000000, 0.8191520442889952403, -0.5735764363510413855 ) ) ;
#12855 = DIRECTION ( 'NONE',  ( 1.000000000000000000, 0.000000000000000000, 1.224646799147353207E-16 ) ) ;
#12856 = CARTESIAN_POINT ( 'NONE',  ( -5.577813053751546416E-15, -25.38624068961733826, -5.000041789647243107 ) ) ;
#12857 = CARTESIAN_POINT ( 'NONE',  ( -1.071796769724496334, -29.07582628914216727, -10.26931610931310246 ) ) ;
#12858 = CARTESIAN_POINT ( 'NONE',  ( -1.661723472263481630E-14, -20.25262601527420969, -11.61605459007084029 ) ) ;
#12859 = CARTESIAN_POINT ( 'NONE',  ( 4.243569643750000786, -21.70633658100450702, -6.718381254414091508 ) ) ;
#12860 = ORIENTED_EDGE ( 'NONE', *, *, #11743, .F. ) ;
#12861 = CARTESIAN_POINT ( 'NONE',  ( 0.000000000000000000, 43.00000000000000000, 0.000000000000000000 ) ) ;
#12862 = EDGE_LOOP ( 'NONE', ( #2506, #12803 ) ) ;
#12863 = ORIENTED_EDGE ( 'NONE', *, *, #17964, .F. ) ;
#12864 = DIRECTION ( 'NONE',  ( -0.000000000000000000, -1.000000000000000000, -0.000000000000000000 ) ) ;
#12865 = DIRECTION ( 'NONE',  ( -1.000000000000000000, -0.000000000000000000, -0.000000000000000000 ) ) ;
#12866 = CARTESIAN_POINT ( 'NONE',  ( -0.05938372350918959958, 16.37819992234354416, 4.731580009072201776 ) ) ;
#12867 = CARTESIAN_POINT ( 'NONE',  ( 2.211161402132839182, 30.37819992234354416, -2.942372952327217739 ) ) ;
#12868 = CARTESIAN_POINT ( 'NONE',  ( 0.05938372350926800214, 39.87180007765647360, 2.628655560595669183 ) ) ;
#12869 = ORIENTED_EDGE ( 'NONE', *, *, #17223, .F. ) ;
#12870 = CARTESIAN_POINT ( 'NONE',  ( 2.733110507866328920, 31.12819992234354416, 3.862833514489095510 ) ) ;
#12871 = EDGE_CURVE ( 'NONE', #8755, #3130, #11485, .T. ) ;
#12872 = CARTESIAN_POINT ( 'NONE',  ( -1.999999999999996225, -20.15388036368618074, -10.54072086271434117 ) ) ;
#12873 = EDGE_LOOP ( 'NONE', ( #14653, #13221, #9291, #11675 ) ) ;
#12874 = ADVANCED_FACE ( 'NONE', ( #12796 ), #255, .T. ) ;
#12875 = CARTESIAN_POINT ( 'NONE',  ( 2.211161402132902243, 27.12180007765647360, 2.942372952327172442 ) ) ;
#12876 = EDGE_CURVE ( 'NONE', #3700, #4080, #14783, .T. ) ;
#12877 = CARTESIAN_POINT ( 'NONE',  ( -9.890239780389581625, -9.933741096495946721, 2.532703114057662575 ) ) ;
#12878 = CARTESIAN_POINT ( 'NONE',  ( 4.243569643749997233, -23.96063528801558462, -5.666363347791923744 ) ) ;
#12879 = EDGE_CURVE ( 'NONE', #5337, #13588, #12974, .T. ) ;
#12880 = CARTESIAN_POINT ( 'NONE',  ( 1.444289557196047680, 34.74680007765647360, 4.262301884875704161 ) ) ;
#12881 = EDGE_CURVE ( 'NONE', #12502, #18310, #16202, .T. ) ;
#12882 = DIRECTION ( 'NONE',  ( 0.000000000000000000, 0.000000000000000000, 1.000000000000000000 ) ) ;
#12883 = ORIENTED_EDGE ( 'NONE', *, *, #2547, .T. ) ;
#12884 = ORIENTED_EDGE ( 'NONE', *, *, #15940, .F. ) ;
#12885 = CARTESIAN_POINT ( 'NONE',  ( -1.027846397803541700, 27.49680007765648071, 3.346150245485522312 ) ) ;
#12886 = CARTESIAN_POINT ( 'NONE',  ( -3.999999999999997335, -21.33635595023595144, -10.21631206112735057 ) ) ;
#12887 = CARTESIAN_POINT ( 'NONE',  ( -1.734723475976807094E-15, 16.59999999999999787, -2.500000000000000000 ) ) ;
#12888 = CARTESIAN_POINT ( 'NONE',  ( -1.734723475976807094E-15, 27.59999999999999432, -2.500000000000000000 ) ) ;
#12889 = EDGE_LOOP ( 'NONE', ( #6912, #5821, #7116, #8226 ) ) ;
#12890 = CARTESIAN_POINT ( 'NONE',  ( 2.864755990943222308, 20.50319992234354416, -2.011557305968548093 ) ) ;
#12891 = DIRECTION ( 'NONE',  ( 0.000000000000000000, 0.8191520442889949072, -0.5735764363510414965 ) ) ;
#12892 = CARTESIAN_POINT ( 'NONE',  ( 2.121784821874994176, -26.53427271694390299, -7.206153456172153859 ) ) ;
#12893 = CARTESIAN_POINT ( 'NONE',  ( 2.115076519116362963, 36.37180007765648782, -3.012182706137107147 ) ) ;
#12894 = CARTESIAN_POINT ( 'NONE',  ( -3.500000000000000444, 32.00319992234354771, -0.05647727720529563400 ) ) ;
#12895 = CYLINDRICAL_SURFACE ( 'NONE', #11706, 7.499999999999999112 ) ;
#12896 = CARTESIAN_POINT ( 'NONE',  ( 4.000000000000003553, -25.29403336105814404, -15.86846116672141527 ) ) ;
#12897 = AXIS2_PLACEMENT_3D ( 'NONE', #8357, #2632, #8083 ) ;
#12898 = CARTESIAN_POINT ( 'NONE',  ( -5.330712181944245322E-15, -26.30097046047931997, -4.737218247813111738 ) ) ;
#12899 = CIRCLE ( 'NONE', #175, 0.9999999999999991118 ) ;
#12900 = FACE_OUTER_BOUND ( 'NONE', #15591, .T. ) ;
#12901 = DIRECTION ( 'NONE',  ( -0.000000000000000000, -1.000000000000000000, -0.000000000000000000 ) ) ;
#12902 = DIRECTION ( 'NONE',  ( 0.000000000000000000, 1.000000000000000000, 0.000000000000000000 ) ) ;
#12903 = DIRECTION ( 'NONE',  ( 0.000000000000000000, -1.000000000000000000, 1.478898702612462246E-15 ) ) ;
#12904 = CARTESIAN_POINT ( 'NONE',  ( -2.121784821875005722, -23.73808758973257227, -3.212787240263307531 ) ) ;
#12905 = CYLINDRICAL_SURFACE ( 'NONE', #3837, 2.149999999999995470 ) ;
#12906 = FILL_AREA_STYLE ('',( #8290 ) ) ;
#12907 = VERTEX_POINT ( 'NONE', #15965 ) ;
#12908 = CARTESIAN_POINT ( 'NONE',  ( 2.500000000000001332, 20.75319992234354771, 0.05647727720530566764 ) ) ;
#12909 = AXIS2_PLACEMENT_3D ( 'NONE', #8470, #14140, #7084 ) ;
#12910 = CARTESIAN_POINT ( 'NONE',  ( 4.243569643750000786, -26.57815143726116602, -13.67605393059374208 ) ) ;
#12911 = DIRECTION ( 'NONE',  ( -1.000000000000000000, 0.000000000000000000, 4.336808689942021680E-16 ) ) ;
#12912 = FACE_OUTER_BOUND ( 'NONE', #3513, .T. ) ;
#12913 = DIRECTION ( 'NONE',  ( 0.000000000000000000, 0.8191520442889952403, -0.5735764363510413855 ) ) ;
#12914 = ADVANCED_FACE ( 'NONE', ( #1970 ), #12690, .T. ) ;
#12915 = ORIENTED_EDGE ( 'NONE', *, *, #4619, .F. ) ;
#12916 = CARTESIAN_POINT ( 'NONE',  ( -4.243569643750000786, -20.02862550467770220, -4.322361524868783889 ) ) ;
#12917 = CARTESIAN_POINT ( 'NONE',  ( 2.864755990943265829, 31.99680007765647716, 2.011557305968487697 ) ) ;
#12918 = CARTESIAN_POINT ( 'NONE',  ( 4.243569643749996345, -28.38075870064580286, -11.97895378909399078 ) ) ;
#12919 = DIRECTION ( 'NONE',  ( 0.000000000000000000, 0.8191520442889952403, -0.5735764363510413855 ) ) ;
#12920 = CIRCLE ( 'NONE', #8468, 0.9999999999999991118 ) ;
#12921 = CARTESIAN_POINT ( 'NONE',  ( 2.121784821874994176, -28.59914788780765704, -10.15510081561253664 ) ) ;
#12922 = DIRECTION ( 'NONE',  ( 0.000000000000000000, 0.8191520442889952403, -0.5735764363510413855 ) ) ;
#12923 = CARTESIAN_POINT ( 'NONE',  ( -3.706921591972381904E-14, -17.99416879784692469, -8.390643416689682610 ) ) ;
#12924 = CARTESIAN_POINT ( 'NONE',  ( 4.000000000000003553, -24.06801372906274139, -14.11752367306044853 ) ) ;
#12925 = CARTESIAN_POINT ( 'NONE',  ( -5.330712181944245322E-15, -28.59169135315628907, -8.008706724692286727 ) ) ;
#12926 = DIRECTION ( 'NONE',  ( 0.000000000000000000, 0.8191520442889952403, -0.5735764363510413855 ) ) ;
#12927 = CARTESIAN_POINT ( 'NONE',  ( -1.999999999999996225, -17.89542314625890285, -7.315309689333185261 ) ) ;
#12928 = CARTESIAN_POINT ( 'NONE',  ( -0.7188294034286043521, 24.99680007765647716, 2.395093729190366005 ) ) ;
#12929 = VERTEX_POINT ( 'NONE', #4454 ) ;
#12930 = CARTESIAN_POINT ( 'NONE',  ( 3.481649420246370141, 24.12180007765648071, -1.193696214020541602 ) ) ;
#12931 = CARTESIAN_POINT ( 'NONE',  ( 2.599319604203554679, -24.48737926485759431, -15.99075565718284153 ) ) ;
#12932 = EDGE_CURVE ( 'NONE', #5635, #2806, #862, .T. ) ;
#12933 = DIRECTION ( 'NONE',  ( 0.000000000000000000, 0.000000000000000000, 1.000000000000000000 ) ) ;
#12934 = FACE_OUTER_BOUND ( 'NONE', #17644, .T. ) ;
#12935 = EDGE_CURVE ( 'NONE', #1567, #1143, #11206, .T. ) ;
#12936 = AXIS2_PLACEMENT_3D ( 'NONE', #8567, #3022, #11350 ) ;
#12937 = CARTESIAN_POINT ( 'NONE',  ( 2.055738996568281518, 33.00319992234354771, -1.423772053676066518 ) ) ;
#12938 = ORIENTED_EDGE ( 'NONE', *, *, #1516, .F. ) ;
#12939 = CARTESIAN_POINT ( 'NONE',  ( -4.243569643750000786, -24.67459463912114259, -10.95749308360964136 ) ) ;
#12940 = EDGE_CURVE ( 'NONE', #3808, #13373, #7411, .T. ) ;
#12941 = CARTESIAN_POINT ( 'NONE',  ( 0.05938372350929014415, 29.87180007765647005, 4.731580009072201776 ) ) ;
#12942 = ORIENTED_EDGE ( 'NONE', *, *, #13924, .T. ) ;
#12943 = ADVANCED_FACE ( 'NONE', ( #386, #7509, #6310 ), #16240, .F. ) ;
#12944 = DIRECTION ( 'NONE',  ( 0.000000000000000000, 1.000000000000000000, 0.000000000000000000 ) ) ;
#12945 = CARTESIAN_POINT ( 'NONE',  ( 1.071796769724476128, -16.71514851677590485, -6.564013151695367476 ) ) ;
#12946 = CARTESIAN_POINT ( 'NONE',  ( 2.121784821874994176, -29.14763035506834044, -10.93841495796388763 ) ) ;
#12947 = CARTESIAN_POINT ( 'NONE',  ( 3.999999999999996447, 6.938893903907228378E-15, 0.000000000000000000 ) ) ;
#12948 = TOROIDAL_SURFACE ( 'NONE', #12356, 9.000000000000001776, 0.9999999999999991118 ) ;
#12949 = FACE_OUTER_BOUND ( 'NONE', #3284, .T. ) ;
#12951 = CARTESIAN_POINT ( 'NONE',  ( -5.577813053751546416E-15, -29.25788163498686245, -10.52931808859795559 ) ) ;
#12950 = CIRCLE ( 'NONE', #11176, 0.2000000000000000944 ) ;
#12952 = CARTESIAN_POINT ( 'NONE',  ( 4.243569643750000786, -21.44822718464654088, -6.349762834484042884 ) ) ;
#12953 = ORIENTED_EDGE ( 'NONE', *, *, #18188, .F. ) ;
#12954 = VERTEX_POINT ( 'NONE', #10838 ) ;
#12955 = EDGE_LOOP ( 'NONE', ( #17275, #3557, #4850 ) ) ;
#12956 = DIRECTION ( 'NONE',  ( 0.000000000000000000, 0.000000000000000000, -1.000000000000000000 ) ) ;
#12957 = DIRECTION ( 'NONE',  ( -3.469446951953613696E-16, -0.000000000000000000, -1.000000000000000000 ) ) ;
#12958 =( NAMED_UNIT ( * ) PLANE_ANGLE_UNIT ( ) SI_UNIT ( $, .RADIAN. ) );
#12959 = CARTESIAN_POINT ( 'NONE',  ( 1.444289557195957086, 17.75319992234354061, -4.262301884875733471 ) ) ;
#12960 = CARTESIAN_POINT ( 'NONE',  ( 1.027846397803612311, 26.25319992234354771, 3.346150245485499219 ) ) ;
#12961 = CARTESIAN_POINT ( 'NONE',  ( 2.518350579753628971, 39.37180007765647360, 0.7558219633769073242 ) ) ;
#12962 = ORIENTED_EDGE ( 'NONE', *, *, #10973, .F. ) ;
#12963 = CIRCLE ( 'NONE', #17131, 2.149999999999995470 ) ;
#12964 = CARTESIAN_POINT ( 'NONE',  ( 2.829195390882724759, 32.87819992234354771, -3.793023760679264278 ) ) ;
#12965 = AXIS2_PLACEMENT_3D ( 'NONE', #4540, #3064, #16992 ) ;
#12966 = CARTESIAN_POINT ( 'NONE',  ( -1.999999999999996225, -20.67009915640211659, -11.27795770257443841 ) ) ;
#12967 = VERTEX_POINT ( 'NONE', #756 ) ;
#12968 = CARTESIAN_POINT ( 'NONE',  ( 8.000000000000000000, 0.000000000000000000, 6.500000000000000000 ) ) ;
#12969 = CARTESIAN_POINT ( 'NONE',  ( 0.05938372350927906274, 29.87180007765648071, 3.680117784833935701 ) ) ;
#12970 = CARTESIAN_POINT ( 'NONE',  ( -7.505322150676213333, -12.67849954855525496, 7.208879555002704720 ) ) ;
#12971 = CARTESIAN_POINT ( 'NONE',  ( -2.121784821875005722, -23.99619698609053842, -3.581405660193354379 ) ) ;
#12972 = CARTESIAN_POINT ( 'NONE',  ( -3.607379964056306676, 32.74680007765648071, 2.690724712371306282 ) ) ;
#12973 = VECTOR ( 'NONE', #17850, 1000.000000000000000 ) ;
#12974 = LINE ( 'NONE', #17181, #5594 ) ;
#12975 = ORIENTED_EDGE ( 'NONE', *, *, #17924, .T. ) ;
#12976 = AXIS2_PLACEMENT_3D ( 'NONE', #1680, #5932, #8609 ) ;
#12977 = EDGE_LOOP ( 'NONE', ( #13217, #2224, #5254, #4348 ) ) ;
#12978 = CARTESIAN_POINT ( 'NONE',  ( -2.798362969681365886, 20.24680007765647716, 2.102939460078824929 ) ) ;
#12979 = LINE ( 'NONE', #17371, #405 ) ;
#12980 =( LENGTH_UNIT ( ) NAMED_UNIT ( * ) SI_UNIT ( .MILLI., .METRE. ) );
#12981 = CARTESIAN_POINT ( 'NONE',  ( 3.999999999999996447, -22.99045465720753256, -4.525974018286417433 ) ) ;
#12982 = CARTESIAN_POINT ( 'NONE',  ( 2.000000000000004441, -22.00366437091829397, -13.18248620554634698 ) ) ;
#12983 = ORIENTED_EDGE ( 'NONE', *, *, #12044, .F. ) ;
#12984 = CARTESIAN_POINT ( 'NONE',  ( -0.05938372350920063936, 18.87819992234354771, 3.680117784833935701 ) ) ;
#12985 = CARTESIAN_POINT ( 'NONE',  ( -2.000000000000005773, -29.16304524001135334, -11.32818800201368781 ) ) ;
#12986 = CARTESIAN_POINT ( 'NONE',  ( 2.121784821875004390, -20.16929524862920431, -10.93049390676413601 ) ) ;
#12987 = CARTESIAN_POINT ( 'NONE',  ( 1.989345975306426206, 16.49680007765648071, -1.515154207786343799 ) ) ;
#12988 =( BOUNDED_CURVE ( )  B_SPLINE_CURVE ( 2, ( #8587, #8968, #1563, #7571, #14644, #11837, #7200, #12857, #164 ),
 .UNSPECIFIED., .F., .F. ) 
 B_SPLINE_CURVE_WITH_KNOTS ( ( 3, 2, 2, 2, 3 ),
 ( 0.1465517241379310498, 0.1494252873563218509, 0.1551724137931034531, 0.1609195402298850552, 0.1637931034482758563 ),
 .UNSPECIFIED. ) 
 CURVE ( )  GEOMETRIC_REPRESENTATION_ITEM ( )  RATIONAL_B_SPLINE_CURVE ( ( 0.9330127018922192983, 0.9330127018922196314, 1.000000000000000000, 0.8660254037844387076, 1.000000000000000000, 0.8660254037844387076, 1.000000000000000000, 0.9330127018922194093, 0.9330127018922194093 ) ) 
 REPRESENTATION_ITEM ( '' )  );
#12989 = CARTESIAN_POINT ( 'NONE',  ( 3.500000000000000444, 35.75319992234354771, 0.05647727720529520379 ) ) ;
#12990 = LINE ( 'NONE', #304, #14079 ) ;
#12991 = LINE ( 'NONE', #7057, #4024 ) ;
#12992 = ADVANCED_FACE ( 'NONE', ( #9179 ), #15967, .T. ) ;
#12993 = VECTOR ( 'NONE', #13413, 999.9999999999998863 ) ;
#12994 = CARTESIAN_POINT ( 'NONE',  ( 4.243569643750000786, -23.25499295915232167, -8.930091773994377036 ) ) ;
#12995 = AXIS2_PLACEMENT_3D ( 'NONE', #10374, #6479, #11955 ) ;
#12996 = DIRECTION ( 'NONE',  ( 0.000000000000000000, 0.000000000000000000, 1.000000000000000000 ) ) ;
#12997 = CARTESIAN_POINT ( 'NONE',  ( -3.537103074283056703, -10.00000000000000178, -11.53856502750640978 ) ) ;
#12998 = CARTESIAN_POINT ( 'NONE',  ( -1.071796769724496334, -23.91363836198279103, -2.896947710712150403 ) ) ;
#12999 = AXIS2_PLACEMENT_3D ( 'NONE', #2651, #6892, #8103 ) ;
#13000 = VERTEX_POINT ( 'NONE', #3620 ) ;
#13001 = CARTESIAN_POINT ( 'NONE',  ( -4.243569643750005227, -23.27234356439432972, -4.683380894645135406 ) ) ;
#13002 = CARTESIAN_POINT ( 'NONE',  ( 4.000000000000000888, -24.69072647674599352, -10.98053173535865135 ) ) ;
#13003 = FACE_BOUND ( 'NONE', #13981, .T. ) ;
#13004 = ORIENTED_EDGE ( 'NONE', *, *, #6249, .T. ) ;
#13005 = VECTOR ( 'NONE', #17246, 1000.000000000000000 ) ;
#13006 = CARTESIAN_POINT ( 'NONE',  ( 1.593127413382953383, 22.87819992234354771, -2.091722143975172532 ) ) ;
#13007 = CARTESIAN_POINT ( 'NONE',  ( -4.243569643749997233, -24.46366198661064573, -14.92774014801135074 ) ) ;
#13008 = CARTESIAN_POINT ( 'NONE',  ( 2.798362969681366330, 16.49680007765647716, -2.102939460078824929 ) ) ;
#13009 = CARTESIAN_POINT ( 'NONE',  ( 4.481649420246366589, 16.62180007765647716, -1.518615910253458212 ) ) ;
#13010 = DIRECTION ( 'NONE',  ( -0.000000000000000000, -1.000000000000000000, -0.000000000000000000 ) ) ;
#13011 = ADVANCED_FACE ( 'NONE', ( #12228 ), #14858, .F. ) ;
#13012 = CARTESIAN_POINT ( 'NONE',  ( 8.511038526056729836, -10.00000000000000178, -5.033916384140447953 ) ) ;
#13013 = VERTEX_POINT ( 'NONE', #9084 ) ;
#13014 = CARTESIAN_POINT ( 'NONE',  ( 4.243569643750003451, -18.64544601037477278, -6.618466598754856101 ) ) ;
#13015 = CARTESIAN_POINT ( 'NONE',  ( -1.027846397803541700, 39.99680007765648071, 3.346150245485522312 ) ) ;
#13016 = CARTESIAN_POINT ( 'NONE',  ( 2.121784821874994176, -29.92195854414224598, -12.04427021775403084 ) ) ;
#13017 = VECTOR ( 'NONE', #7638, 1000.000000000000000 ) ;
#13018 = CARTESIAN_POINT ( 'NONE',  ( 0.000000000000000000, 9.254131787996968228, 30.52396275209373044 ) ) ;
#13019 = CARTESIAN_POINT ( 'NONE',  ( 2.121784821875004390, -21.97606102313498511, -13.51082284627447017 ) ) ;
#13020 = LINE ( 'NONE', #5971, #14714 ) ;
#13021 = DIRECTION ( 'NONE',  ( 0.000000000000000000, -1.000000000000000000, 0.000000000000000000 ) ) ;
#13022 = FACE_OUTER_BOUND ( 'NONE', #1499, .T. ) ;
#13023 = CARTESIAN_POINT ( 'NONE',  ( -2.121784821875005722, -28.12594732781803941, -9.479300379074118155 ) ) ;
#13024 = DIRECTION ( 'NONE',  ( -1.000000000000000000, 0.000000000000000000, 4.336808689942021680E-16 ) ) ;
#13025 = CARTESIAN_POINT ( 'NONE',  ( -4.000000000000004441, -22.04405353722830085, -3.174373145209581804 ) ) ;
#13026 = CARTESIAN_POINT ( 'NONE',  ( -2.055738996568313048, 25.74680007765648426, -1.423772053676023441 ) ) ;
#13027 = EDGE_LOOP ( 'NONE', ( #1571, #8548, #15779, #13106 ) ) ;
#13028 = CARTESIAN_POINT ( 'NONE',  ( 3.500000000000000444, 19.24680007765648071, -0.05647727720536935281 ) ) ;
#13029 = DIRECTION ( 'NONE',  ( -3.373073425510457965E-16, 0.000000000000000000, -1.000000000000000000 ) ) ;
#13030 = DIRECTION ( 'NONE',  ( 0.000000000000000000, 0.000000000000000000, 1.000000000000000000 ) ) ;
#13031 = AXIS2_PLACEMENT_3D ( 'NONE', #16264, #3553, #4753 ) ;
#13032 = DIRECTION ( 'NONE',  ( -0.000000000000000000, -1.000000000000000000, -0.000000000000000000 ) ) ;
#13033 = CARTESIAN_POINT ( 'NONE',  ( 2.211161402132839626, 17.87819992234354771, -2.942372952327218183 ) ) ;
#13034 = EDGE_LOOP ( 'NONE', ( #738, #7994, #6196, #8703 ) ) ;
#13035 = CARTESIAN_POINT ( 'NONE',  ( -2.121784821875005722, -26.86766402057294556, -7.682285581915135886 ) ) ;
#13036 = CARTESIAN_POINT ( 'NONE',  ( 3.607379964056306676, 31.49680007765647716, -2.690724712371305838 ) ) ;
#13037 = VERTEX_POINT ( 'NONE', #12047 ) ;
#13038 = CARTESIAN_POINT ( 'NONE',  ( 1.071796769724476128, -18.19927754512928075, -8.683569065286379285 ) ) ;
#13039 = EDGE_CURVE ( 'NONE', #6854, #15972, #4394, .T. ) ;
#13040 = CARTESIAN_POINT ( 'NONE',  ( 4.730628863548789710E-15, -21.49956243961515767, -14.96605739982588368 ) ) ;
#13041 = DIRECTION ( 'NONE',  ( 0.000000000000000000, 1.000000000000000000, 0.000000000000000000 ) ) ;
#13042 = AXIS2_PLACEMENT_3D ( 'NONE', #5527, #9960, #2582 ) ;
#13043 = DIRECTION ( 'NONE',  ( -1.000000000000000000, -0.000000000000000000, -0.000000000000000000 ) ) ;
#13044 = EDGE_CURVE ( 'NONE', #3510, #13645, #3793, .T. ) ;
#13045 = CARTESIAN_POINT ( 'NONE',  ( 0.000000000000000000, 7.715274834628324392E-16, -6.099999999999999645 ) ) ;
#13046 = CARTESIAN_POINT ( 'NONE',  ( -4.243569643750005227, -23.30460723893907371, -4.729458197136391817 ) ) ;
#13047 = ORIENTED_EDGE ( 'NONE', *, *, #6799, .F. ) ;
#13049 = ADVANCED_FACE ( 'NONE', ( #6215 ), #3523, .T. ) ;
#13048 = CARTESIAN_POINT ( 'NONE',  ( 1.999999999999994449, -23.89331173033122369, -3.802228594101777492 ) ) ;
#13050 = CARTESIAN_POINT ( 'NONE',  ( -3.706921591972381904E-14, -19.73640722255826319, -10.87881775021074127 ) ) ;
#13051 = ORIENTED_EDGE ( 'NONE', *, *, #2280, .F. ) ;
#13052 = EDGE_LOOP ( 'NONE', ( #10007, #17748, #8219, #7292 ) ) ;
#13053 = CARTESIAN_POINT ( 'NONE',  ( -4.000000000000004441, -22.30216293358627055, -3.542991565139629984 ) ) ;
#13054 = DIRECTION ( 'NONE',  ( 1.000000000000000000, 0.000000000000000000, 0.000000000000000000 ) ) ;
#13055 = FILL_AREA_STYLE ('',( #15755 ) ) ;
#13056 = EDGE_CURVE ( 'NONE', #7716, #10740, #7407, .T. ) ;
#13057 = CARTESIAN_POINT ( 'NONE',  ( 4.499999999999999112, 25.75319992234354771, 0.05647727720528474687 ) ) ;
#13058 = CARTESIAN_POINT ( 'NONE',  ( 0.05938372350920110426, 30.12819992234354416, -3.680117784833935701 ) ) ;
#13059 = CARTESIAN_POINT ( 'NONE',  ( 1.989345975306457071, 16.00319992234354771, 1.515154207786300500 ) ) ;
#13060 = ORIENTED_EDGE ( 'NONE', *, *, #10565, .T. ) ;
#13061 = CARTESIAN_POINT ( 'NONE',  ( -0.05938372350918959958, 31.37819992234354061, 4.731580009072201776 ) ) ;
#13062 = CARTESIAN_POINT ( 'NONE',  ( 1.999999999999994449, -25.18385871212106863, -5.645320693752015728 ) ) ;
#13063 = ORIENTED_EDGE ( 'NONE', *, *, #7156, .F. ) ;
#13064 = CARTESIAN_POINT ( 'NONE',  ( 9.530870139287183087E-15, 13.00000000000000178, 7.000000000000003553 ) ) ;
#13065 = CARTESIAN_POINT ( 'NONE',  ( -2.211161402132902243, 30.87180007765647716, -2.942372952327172886 ) ) ;
#13066 = CARTESIAN_POINT ( 'NONE',  ( 9.911039980157271501, -9.932630671411386558, 2.546919849226038313 ) ) ;
#13067 = CARTESIAN_POINT ( 'NONE',  ( 4.243569643750000786, -21.15785411374382363, -5.935067112062737849 ) ) ;
#13068 = AXIS2_PLACEMENT_3D ( 'NONE', #2362, #5490, #7991 ) ;
#13069 = CARTESIAN_POINT ( 'NONE',  ( 3.673772985318219053, 31.99680007765648071, 2.599342558260951730 ) ) ;
#13070 = DIRECTION ( 'NONE',  ( 0.000000000000000000, -1.000000000000000000, 9.859324684083080328E-16 ) ) ;
#13071 = EDGE_LOOP ( 'NONE', ( #11654, #16448, #2677, #10775, #8086 ) ) ;
#13072 = CARTESIAN_POINT ( 'NONE',  ( -3.481649420246369697, 30.37180007765647005, 1.193696214020542490 ) ) ;
#13073 = DIRECTION ( 'NONE',  ( -1.000000000000000000, -0.000000000000000000, -0.000000000000000000 ) ) ;
#13074 = FACE_OUTER_BOUND ( 'NONE', #552, .T. ) ;
#13075 = CARTESIAN_POINT ( 'NONE',  ( 9.000000000000005329, 34.19999999999999574, 2.499999999999997335 ) ) ;
#13076 = EDGE_LOOP ( 'NONE', ( #9463, #7034, #6814, #16578 ) ) ;
#13077 = CARTESIAN_POINT ( 'NONE',  ( -3.481649420246394122, 24.62819992234354061, -1.193696214020467883 ) ) ;
#13078 = CARTESIAN_POINT ( 'NONE',  ( 1.071796769724495224, -22.39355523665122405, -14.67361839015640967 ) ) ;
#13079 = CARTESIAN_POINT ( 'NONE',  ( 4.243569643750003451, -19.12940112854596819, -7.309626136123695161 ) ) ;
#13080 = CARTESIAN_POINT ( 'NONE',  ( -3.500000000000000444, 35.49680007765648071, 0.05647727720536892260 ) ) ;
#13081 = AXIS2_PLACEMENT_3D ( 'NONE', #15969, #13073, #3261 ) ;
#13082 = CARTESIAN_POINT ( 'NONE',  ( -2.864755990943222308, 31.75319992234354416, 2.011557305968548093 ) ) ;
#13083 = AXIS2_PLACEMENT_3D ( 'NONE', #16914, #17187, #15688 ) ;
#13084 = DIRECTION ( 'NONE',  ( 0.000000000000000000, 0.000000000000000000, -1.000000000000000000 ) ) ;
#13085 = CARTESIAN_POINT ( 'NONE',  ( 4.000000000000000888, -26.94918369417327142, -14.20594290873980192 ) ) ;
#13086 = PRODUCT_DEFINITION_FORMATION_WITH_SPECIFIED_SOURCE ( 'ANY', '', #16425, .NOT_KNOWN. ) ;
#13087 = CARTESIAN_POINT ( 'NONE',  ( -4.243569643750000786, -22.09350067554145625, -7.271308884309165776 ) ) ;
#13088 = EDGE_CURVE ( 'NONE', #15568, #8704, #438, .T. ) ;
#13089 = CARTESIAN_POINT ( 'NONE',  ( 0.000000000000000000, 9.254131787996968228, 30.52396275209373044 ) ) ;
#13090 = CARTESIAN_POINT ( 'NONE',  ( -1.734723475976807094E-15, 34.19999999999999574, -2.500000000000000000 ) ) ;
#13091 = CARTESIAN_POINT ( 'NONE',  ( 14.99999999999999822, 13.00000000000000178, -25.00000000000000355 ) ) ;
#13092 = CIRCLE ( 'NONE', #5702, 0.9999999999999991118 ) ;
#13093 = DIRECTION ( 'NONE',  ( 0.000000000000000000, 0.000000000000000000, 1.000000000000000000 ) ) ;
#13094 = ORIENTED_EDGE ( 'NONE', *, *, #14664, .T. ) ;
#13095 = EDGE_LOOP ( 'NONE', ( #4778, #15712, #8667, #3818 ) ) ;
#13096 =( BOUNDED_CURVE ( )  B_SPLINE_CURVE ( 2, ( #9870, #16582, #10907, #16767, #9509, #11260, #11081, #7085, #15463 ),
 .UNSPECIFIED., .F., .T. ) 
 B_SPLINE_CURVE_WITH_KNOTS ( ( 3, 2, 2, 2, 3 ),
 ( 0.6293103448275861878, 0.6321839080459770166, 0.6379310344827586743, 0.6436781609195402210, 0.6465517241379310498 ),
 .UNSPECIFIED. ) 
 CURVE ( )  GEOMETRIC_REPRESENTATION_ITEM ( )  RATIONAL_B_SPLINE_CURVE ( ( 0.9330127018922194093, 0.9330127018922194093, 1.000000000000000000, 0.8660254037844387076, 1.000000000000000000, 0.8660254037844387076, 1.000000000000000000, 0.9330127018922194093, 0.9330127018922194093 ) ) 
 REPRESENTATION_ITEM ( '' )  );
#13097 = CARTESIAN_POINT ( 'NONE',  ( -4.243569643749997233, -17.75281768130346194, -5.343661229830111381 ) ) ;
#13098 = CARTESIAN_POINT ( 'NONE',  ( 6.123233995736766282E-16, 15.00000000000000355, -5.000000000000000000 ) ) ;
#13099 = CARTESIAN_POINT ( 'NONE',  ( 0.000000000000000000, -1.443375672974064328, 1.278502688459867223E-18 ) ) ;
#13100 = EDGE_LOOP ( 'NONE', ( #5118, #3857 ) ) ;
#13101 = CARTESIAN_POINT ( 'NONE',  ( -1.989345975306457071, 22.25319992234354771, -1.515154207786300944 ) ) ;
#13102 = CARTESIAN_POINT ( 'NONE',  ( 2.121784821875004390, -22.49227981585092095, -14.24805968613456564 ) ) ;
#13103 = CARTESIAN_POINT ( 'NONE',  ( -0.05938372350927861171, 16.12180007765647716, -3.680117784833935701 ) ) ;
#13104 = CARTESIAN_POINT ( 'NONE',  ( 4.898587196589413815E-16, 2.700915433685006750, 35.11257424290206330 ) ) ;
#13105 = CARTESIAN_POINT ( 'NONE',  ( 2.649389826666416869, -10.00000000000053824, -4.175485738721015139 ) ) ;
#13106 = ORIENTED_EDGE ( 'NONE', *, *, #1841, .T. ) ;
#13107 = CIRCLE ( 'NONE', #8657, 3.799999999999999378 ) ;
#13108 = CARTESIAN_POINT ( 'NONE',  ( -1.135272562821090014, 38.49680007765647360, -3.311245368580554072 ) ) ;
#13109 = PRESENTATION_LAYER_ASSIGNMENT (  '', '', ( #6603 ) ) ;
#13110 = CARTESIAN_POINT ( 'NONE',  ( -2.121784821875005722, -29.70686738051060161, -11.73708820114566009 ) ) ;
#13111 = EDGE_CURVE ( 'NONE', #15867, #9076, #9959, .T. ) ;
#13112 = FILL_AREA_STYLE ('',( #14519 ) ) ;
#13113 = CARTESIAN_POINT ( 'NONE',  ( 4.243569643750003451, -23.77537026298940503, -13.94475769486455263 ) ) ;
#13114 = CARTESIAN_POINT ( 'NONE',  ( -1.734723475976807094E-15, 18.79999999999999361, -2.500000000000000000 ) ) ;
#13115 = EDGE_CURVE ( 'NONE', #5913, #17692, #9134, .T. ) ;
#13116 = DIRECTION ( 'NONE',  ( 0.000000000000000000, 0.000000000000000000, -1.000000000000000000 ) ) ;
#13117 = EDGE_CURVE ( 'NONE', #15292, #17585, #7016, .T. ) ;
#13118 = CARTESIAN_POINT ( 'NONE',  ( -8.000000000000001776, 27.59999999999999432, 2.499999999999995115 ) ) ;
#13119 = CARTESIAN_POINT ( 'NONE',  ( 2.121784821874994176, -27.82481969873374794, -9.049245555822391651 ) ) ;
#13120 = CARTESIAN_POINT ( 'NONE',  ( 1.071796769724495224, -18.52191429128169631, -9.144342091205695411 ) ) ;
#13121 = CARTESIAN_POINT ( 'NONE',  ( -5.279047395330986450E-15, -23.63467652125394025, -1.419700282245455636 ) ) ;
#13122 = CARTESIAN_POINT ( 'NONE',  ( -2.481649420246374138, 25.37180007765648426, 0.8687765177876256573 ) ) ;
#13123 = ORIENTED_EDGE ( 'NONE', *, *, #16535, .F. ) ;
#13124 = CARTESIAN_POINT ( 'NONE',  ( 3.500000000000000444, 24.24680007765647716, -0.05647727720536935281 ) ) ;
#13125 = FACE_OUTER_BOUND ( 'NONE', #14515, .T. ) ;
#13126 = CARTESIAN_POINT ( 'NONE',  ( 2.000000000000004441, -23.61684809886054381, -15.48635133111591067 ) ) ;
#13127 = CARTESIAN_POINT ( 'NONE',  ( -5.000000000000001776, 0.000000000000000000, 5.000000000000000888 ) ) ;
#13128 = CARTESIAN_POINT ( 'NONE',  ( -3.481649420246394122, 22.12819992234353705, -1.193696214020467883 ) ) ;
#13129 = VERTEX_POINT ( 'NONE', #1212 ) ;
#13130 = CARTESIAN_POINT ( 'NONE',  ( -2.121784821874996396, -21.70719706859543408, -13.12684532551400629 ) ) ;
#13131 = CARTESIAN_POINT ( 'NONE',  ( -3.500000000000000444, 15.49680007765647893, 0.05647727720536892260 ) ) ;
#13132 = ORIENTED_EDGE ( 'NONE', *, *, #15462, .T. ) ;
#13133 = VECTOR ( 'NONE', #13384, 1000.000000000000000 ) ;
#13134 = CARTESIAN_POINT ( 'NONE',  ( -9.000000000000001776, 34.19999999999999574, 2.499999999999995559 ) ) ;
#13135 = CARTESIAN_POINT ( 'NONE',  ( 0.000000000000000000, 40.79999999999999716, 2.500000000000000000 ) ) ;
#13136 = CARTESIAN_POINT ( 'NONE',  ( 4.243569643749996345, -27.60643051157189731, -10.87309852930384935 ) ) ;
#13137 = DIRECTION ( 'NONE',  ( -1.000000000000000000, -0.000000000000000000, -0.000000000000000000 ) ) ;
#13138 = CARTESIAN_POINT ( 'NONE',  ( 1.820000000000000062, -3.799999999999999378, -4.653657836759940757E-16 ) ) ;
#13139 = DIRECTION ( 'NONE',  ( 0.000000000000000000, 0.000000000000000000, 1.000000000000000000 ) ) ;
#13140 = CARTESIAN_POINT ( 'NONE',  ( -4.243569643750005227, -24.07893542801298281, -5.835313456926535025 ) ) ;
#13141 = ORIENTED_EDGE ( 'NONE', *, *, #14785, .T. ) ;
#13142 = CARTESIAN_POINT ( 'NONE',  ( -4.000000000000000888, -24.81978117492496949, -11.16484094532367699 ) ) ;
#13143 = CARTESIAN_POINT ( 'NONE',  ( -1.734723475976807094E-15, 40.79999999999999716, -12.50000000000000000 ) ) ;
#13144 = FACE_OUTER_BOUND ( 'NONE', #5259, .T. ) ;
#13145 = ORIENTED_EDGE ( 'NONE', *, *, #9727, .T. ) ;
#13146 = EDGE_LOOP ( 'NONE', ( #4266, #17055, #9270, #14379 ) ) ;
#13147 = LINE ( 'NONE', #3241, #8064 ) ;
#13148 = CARTESIAN_POINT ( 'NONE',  ( -8.000000000000001776, 31.99999999999999289, 2.499999999999995115 ) ) ;
#13149 = CARTESIAN_POINT ( 'NONE',  ( -2.829195390882724315, 26.62819992234354416, 3.793023760679264722 ) ) ;
#13150 = CARTESIAN_POINT ( 'NONE',  ( -1.027846397803611866, 27.50319992234354771, -3.346150245485499219 ) ) ;
#13151 = CARTESIAN_POINT ( 'NONE',  ( -1.593127413382952939, 21.62819992234354416, 2.091722143975172532 ) ) ;
#13152 = ORIENTED_EDGE ( 'NONE', *, *, #3601, .F. ) ;
#13153 = CARTESIAN_POINT ( 'NONE',  ( 2.829195390882805583, 17.12180007765647716, 3.793023760679204770 ) ) ;
#13154 = CARTESIAN_POINT ( 'NONE',  ( 2.000000000000004441, -19.93878920005454347, -10.23353884610596509 ) ) ;
#13155 = ORIENTED_EDGE ( 'NONE', *, *, #6880, .T. ) ;
#13156 = ADVANCED_FACE ( 'NONE', ( #15216 ), #12501, .T. ) ;
#13157 = LINE ( 'NONE', #7589, #4122 ) ;
#13158 = CARTESIAN_POINT ( 'NONE',  ( -3.518350579753630747, 33.12180007765646650, -1.080741659609802729 ) ) ;
#13159 = CARTESIAN_POINT ( 'NONE',  ( 4.000000000000003553, -23.48726758655235969, -13.28813222721107934 ) ) ;
#13160 = CARTESIAN_POINT ( 'NONE',  ( 4.243569643749997233, -23.70252589165762203, -5.297744927861876896 ) ) ;
#13161 = CARTESIAN_POINT ( 'NONE',  ( 4.481649420246366589, 29.12180007765647005, -1.518615910253458212 ) ) ;
#13162 = CARTESIAN_POINT ( 'NONE',  ( 4.000000000000003553, -18.06697026303501730, -5.547145408680076883 ) ) ;
#13163 = VERTEX_POINT ( 'NONE', #8145 ) ;
#13164 = CARTESIAN_POINT ( 'NONE',  ( -3.518350579753630747, 33.12180007765646650, -1.080741659609802729 ) ) ;
#13165 = DIRECTION ( 'NONE',  ( -0.000000000000000000, -0.5735764363510414965, -0.8191520442889950182 ) ) ;
#13166 = DIRECTION ( 'NONE',  ( 0.000000000000000000, 0.000000000000000000, 1.000000000000000000 ) ) ;
#13167 = CARTESIAN_POINT ( 'NONE',  ( -1.071796769724486786, -23.33841207085099612, -16.02301379457549757 ) ) ;
#13168 = ORIENTED_EDGE ( 'NONE', *, *, #3440, .F. ) ;
#13169 = CARTESIAN_POINT ( 'NONE',  ( 2.211161402132839626, 25.37819992234353705, -2.942372952327218183 ) ) ;
#13170 = DIRECTION ( 'NONE',  ( 0.000000000000000000, 0.000000000000000000, 1.000000000000000000 ) ) ;
#13171 = CARTESIAN_POINT ( 'NONE',  ( 2.121784821875004390, -17.84631068140748766, -7.612928127393706390 ) ) ;
#13172 = CARTESIAN_POINT ( 'NONE',  ( 0.7188294034286049072, 23.74680007765648426, -2.395093729190366005 ) ) ;
#13173 = EDGE_CURVE ( 'NONE', #17672, #13234, #10317, .T. ) ;
#13174 = EDGE_CURVE ( 'NONE', #2685, #3667, #4163, .T. ) ;
#13175 = CARTESIAN_POINT ( 'NONE',  ( -2.864755990943222308, 36.75319992234354061, 2.011557305968548093 ) ) ;
#13176 = CARTESIAN_POINT ( 'NONE',  ( 2.121784821875004390, -23.55698107582754730, -15.76861066834601210 ) ) ;
#13177 = EDGE_CURVE ( 'NONE', #6640, #14789, #4697, .T. ) ;
#13178 = CARTESIAN_POINT ( 'NONE',  ( 4.000000000000000888, -26.43296490145733557, -13.46870606887970645 ) ) ;
#13179 = CARTESIAN_POINT ( 'NONE',  ( 2.121784821875004390, -18.65290254502614431, -8.764860689675106897 ) ) ;
#13180 = CARTESIAN_POINT ( 'NONE',  ( -6.938893903907228378E-15, 6.938893903907228378E-15, 30.00000000000000000 ) ) ;
#13181 = DIRECTION ( 'NONE',  ( 0.000000000000000000, 0.000000000000000000, 1.000000000000000000 ) ) ;
#13182 = DIRECTION ( 'NONE',  ( 3.469446951953612217E-16, -0.000000000000000000, 1.000000000000000000 ) ) ;
#13183 = DIRECTION ( 'NONE',  ( -1.000000000000000000, 0.000000000000000000, 4.336808689942021680E-16 ) ) ;
#13184 = ORIENTED_EDGE ( 'NONE', *, *, #12653, .F. ) ;
#13185 = ORIENTED_EDGE ( 'NONE', *, *, #1744, .T. ) ;
#13186 = CARTESIAN_POINT ( 'NONE',  ( -4.243569643750005227, -21.72368718624651507, -2.471670375064849434 ) ) ;
#13187 = CARTESIAN_POINT ( 'NONE',  ( -1.734723475976807094E-15, 16.59999999999999787, -2.500000000000000000 ) ) ;
#13188 = VERTEX_POINT ( 'NONE', #18008 ) ;
#13189 = CARTESIAN_POINT ( 'NONE',  ( 1.989345975306457071, 26.00319992234354771, 1.515154207786300500 ) ) ;
#13190 = DIRECTION ( 'NONE',  ( 0.000000000000000000, 0.000000000000000000, 1.000000000000000000 ) ) ;
#13191 = CARTESIAN_POINT ( 'NONE',  ( 4.243569643750000786, -25.54571385182929077, -12.20158025087355114 ) ) ;
#13192 = CARTESIAN_POINT ( 'NONE',  ( -3.481649420246369697, 20.37180007765647716, 1.193696214020542490 ) ) ;
#13193 = VECTOR ( 'NONE', #8271, 1000.000000000000000 ) ;
#13194 = FACE_OUTER_BOUND ( 'NONE', #14252, .T. ) ;
#13195 = CIRCLE ( 'NONE', #8750, 6.500000000000000000 ) ;
#13196 = CARTESIAN_POINT ( 'NONE',  ( 0.3267727178447701331, -10.00000000000000178, -5.052762561672880182 ) ) ;
#13197 = EDGE_LOOP ( 'NONE', ( #15548, #12241, #6447, #12657 ) ) ;
#13198 = DIRECTION ( 'NONE',  ( 0.000000000000000000, 0.000000000000000000, -1.000000000000000000 ) ) ;
#13199 = CARTESIAN_POINT ( 'NONE',  ( -2.121784821874996396, -23.51396284310121487, -15.70717426502434044 ) ) ;
#13200 = EDGE_CURVE ( 'NONE', #11449, #851, #6754, .T. ) ;
#13201 = CARTESIAN_POINT ( 'NONE',  ( -5.330712181944246111E-15, -28.07547256044034967, -7.271469884832190367 ) ) ;
#13202 =( BOUNDED_CURVE ( )  B_SPLINE_CURVE ( 2, ( #4070, #6853, #11468, #4340, #16891, #5823, #5646, #9987, #11289 ),
 .UNSPECIFIED., .F., .F. ) 
 B_SPLINE_CURVE_WITH_KNOTS ( ( 3, 2, 2, 2, 3 ),
 ( 0.1810344827586206906, 0.1839080459770114917, 0.1896551724137930939, 0.1954022988505747238, 0.1982758620689655249 ),
 .UNSPECIFIED. ) 
 CURVE ( )  GEOMETRIC_REPRESENTATION_ITEM ( )  RATIONAL_B_SPLINE_CURVE ( ( 0.9330127018922194093, 0.9330127018922194093, 1.000000000000000000, 0.8660254037844387076, 1.000000000000000000, 0.8660254037844387076, 1.000000000000000000, 0.9330127018922194093, 0.9330127018922194093 ) ) 
 REPRESENTATION_ITEM ( '' )  );
#13203 = DIRECTION ( 'NONE',  ( 0.000000000000000000, 0.000000000000000000, 1.000000000000000000 ) ) ;
#13204 = AXIS2_PLACEMENT_3D ( 'NONE', #14925, #17804, #5159 ) ;
#13205 = CARTESIAN_POINT ( 'NONE',  ( 2.121784821874994176, -25.75994452787000100, -6.100298196382009763 ) ) ;
#13206 = DIRECTION ( 'NONE',  ( -3.469446951953613696E-16, -0.000000000000000000, -1.000000000000000000 ) ) ;
#13207 = DIRECTION ( 'NONE',  ( 1.049727191973305394E-16, 0.5150380737757255245, -0.8571673013836856869 ) ) ;
#13208 = CARTESIAN_POINT ( 'NONE',  ( -2.518350579753628526, 33.12180007765648071, -0.7558219633769075463 ) ) ;
#13209 = DIRECTION ( 'NONE',  ( -0.000000000000000000, -0.5735764363510414965, -0.8191520442889950182 ) ) ;
#13210 = CARTESIAN_POINT ( 'NONE',  ( -1.027846397803541700, 22.49680007765648071, 3.346150245485522312 ) ) ;
#13211 = CARTESIAN_POINT ( 'NONE',  ( 1.999999999999994449, -26.79704244006331493, -7.949185819321580304 ) ) ;
#13212 = CARTESIAN_POINT ( 'NONE',  ( 0.000000000000000000, 0.000000000000000000, 0.000000000000000000 ) ) ;
#13213 = CARTESIAN_POINT ( 'NONE',  ( -1.999999999999996225, -22.54139228070233614, -13.95044124807404451 ) ) ;
#13214 = FACE_OUTER_BOUND ( 'NONE', #16497, .T. ) ;
#13215 = CARTESIAN_POINT ( 'NONE',  ( -3.500000000000000444, 19.50319992234354416, -0.05647727720529563400 ) ) ;
#13216 = EDGE_CURVE ( 'NONE', #4578, #6687, #11162, .T. ) ;
#13217 = ORIENTED_EDGE ( 'NONE', *, *, #13512, .F. ) ;
#13218 = CARTESIAN_POINT ( 'NONE',  ( -4.243569643750000786, -23.12593826097332794, -8.745782564029356720 ) ) ;
#13219 = CARTESIAN_POINT ( 'NONE',  ( -1.135272562821090014, 18.49680007765648071, -3.311245368580554072 ) ) ;
#13220 = CIRCLE ( 'NONE', #11747, 4.000000000000000000 ) ;
#13221 = ORIENTED_EDGE ( 'NONE', *, *, #12040, .F. ) ;
#13222 = EDGE_CURVE ( 'NONE', #4161, #2412, #8253, .T. ) ;
#13223 = DIRECTION ( 'NONE',  ( 0.000000000000000000, 0.000000000000000000, 1.000000000000000000 ) ) ;
#13224 = CARTESIAN_POINT ( 'NONE',  ( -8.500000000000010658, 15.00000000000000178, 20.49999999999998934 ) ) ;
#13225 = CARTESIAN_POINT ( 'NONE',  ( -4.243569643750005227, -28.20868576974048025, -11.73320817580729880 ) ) ;
#13226 = CARTESIAN_POINT ( 'NONE',  ( 14.99999999999999822, 10.00000000000000000, 24.99999999999999645 ) ) ;
#13227 = DIRECTION ( 'NONE',  ( 0.000000000000000000, 0.000000000000000000, -1.000000000000000000 ) ) ;
#13228 = CARTESIAN_POINT ( 'NONE',  ( -4.000000000000004441, -26.88360471823526865, -10.08596851789121018 ) ) ;
#13229 = CARTESIAN_POINT ( 'NONE',  ( -2.121784821874996396, -17.31933733050996338, -6.860332186703194779 ) ) ;
#13230 = VERTEX_POINT ( 'NONE', #2604 ) ;
#13231 = CARTESIAN_POINT ( 'NONE',  ( -8.999999999999996447, -10.00000000000000000, -3.713574246709372417 ) ) ;
#13232 = CARTESIAN_POINT ( 'NONE',  ( -1.999999999999996225, -20.21840771348061949, -10.63287546870361666 ) ) ;
#13233 = CARTESIAN_POINT ( 'NONE',  ( 0.000000000000000000, 13.00000000000000178, 0.000000000000000000 ) ) ;
#13234 = VERTEX_POINT ( 'NONE', #16704 ) ;
#13235 = CIRCLE ( 'NONE', #5245, 0.9999999999999991118 ) ;
#13236 = ORIENTED_EDGE ( 'NONE', *, *, #15717, .T. ) ;
#13237 = CARTESIAN_POINT ( 'NONE',  ( -8.500000000000010658, 15.00000000000000178, 22.64999999999998437 ) ) ;
#13238 = FACE_OUTER_BOUND ( 'NONE', #11452, .T. ) ;
#13239 = SURFACE_STYLE_USAGE ( .BOTH. , #8686 ) ;
#13240 = CARTESIAN_POINT ( 'NONE',  ( 4.518350579753602325, 23.12819992234354416, -1.405661355842793725 ) ) ;
#13241 = CARTESIAN_POINT ( 'NONE',  ( 1.135272562821020070, 37.75319992234354061, -3.311245368580577164 ) ) ;
#13242 = CARTESIAN_POINT ( 'NONE',  ( -1.989345975306457071, 17.25319992234354416, -1.515154207786300944 ) ) ;
#13243 = ORIENTED_EDGE ( 'NONE', *, *, #15905, .F. ) ;
#13244 = CARTESIAN_POINT ( 'NONE',  ( 2.829195390882724759, 37.87819992234353350, -3.793023760679264278 ) ) ;
#13245 = EDGE_CURVE ( 'NONE', #16617, #13, #8790, .T. ) ;
#13246 = CARTESIAN_POINT ( 'NONE',  ( 2.000000000000004441, -19.16446101098063792, -9.127683586315821884 ) ) ;
#13247 = ORIENTED_EDGE ( 'NONE', *, *, #5020, .T. ) ;
#13248 = CARTESIAN_POINT ( 'NONE',  ( 0.3999999999999975797, 0.000000000000000000, 6.099999999999999645 ) ) ;
#13249 = CIRCLE ( 'NONE', #3788, 10.00000000000000000 ) ;
#13250 = CARTESIAN_POINT ( 'NONE',  ( 2.211161402132902243, 32.12180007765647360, 2.942372952327172442 ) ) ;
#13251 = CARTESIAN_POINT ( 'NONE',  ( 3.999999999999996447, -25.76513066735074986, -8.488622031527665257 ) ) ;
#13252 = CARTESIAN_POINT ( 'NONE',  ( 2.121784821874994176, -23.95317875336422020, -3.519969256871676055 ) ) ;
#13253 = CARTESIAN_POINT ( 'NONE',  ( -1.336863392178478716, 27.49680007765647360, 4.297206761780677731 ) ) ;
#13254 = TOROIDAL_SURFACE ( 'NONE', #7333, 9.000000000000001776, 0.9999999999999991118 ) ;
#13255 = CARTESIAN_POINT ( 'NONE',  ( -1.071796769724496334, -26.17209557941007603, -6.122358884093301867 ) ) ;
#13256 = ORIENTED_EDGE ( 'NONE', *, *, #15796, .F. ) ;
#13257 = CARTESIAN_POINT ( 'NONE',  ( -1.287074048710188379, -10.56983422227299130, 22.11683441173179077 ) ) ;
#13258 = DIRECTION ( 'NONE',  ( -1.000000000000000000, 0.000000000000000000, 4.336808689942021680E-16 ) ) ;
#13259 = PRODUCT_DEFINITION_SHAPE ( 'NONE', 'NONE',  #18382 ) ;
#13260 = DIRECTION ( 'NONE',  ( 0.000000000000000000, 0.000000000000000000, 1.000000000000000000 ) ) ;
#13261 =( NAMED_UNIT ( * ) SI_UNIT ( $, .STERADIAN. ) SOLID_ANGLE_UNIT ( ) );
#13262 = EDGE_LOOP ( 'NONE', ( #2287, #17703, #15866 ) ) ;
#13263 = VECTOR ( 'NONE', #13378, 1000.000000000000000 ) ;
#13264 = CARTESIAN_POINT ( 'NONE',  ( -2.864755990943222308, 24.25319992234354416, 2.011557305968548093 ) ) ;
#13265 = CARTESIAN_POINT ( 'NONE',  ( 1.300000000000000044, -1.443375672974064328, 1.278502688459867223E-18 ) ) ;
#13266 = AXIS2_PLACEMENT_3D ( 'NONE', #16446, #7714, #2084 ) ;
#13267 = CARTESIAN_POINT ( 'NONE',  ( 4.243569643750000786, -21.41596351010179333, -6.303685531992786473 ) ) ;
#13268 = CARTESIAN_POINT ( 'NONE',  ( 1.989345975306426206, 18.99680007765647716, -1.515154207786343799 ) ) ;
#13269 = CARTESIAN_POINT ( 'NONE',  ( -0.05938372350918959958, 16.37819992234354416, 4.731580009072201776 ) ) ;
#13270 = CARTESIAN_POINT ( 'NONE',  ( -5.330712181944246111E-15, -30.43072080220681741, -10.63511296669387818 ) ) ;
#13271 = CARTESIAN_POINT ( 'NONE',  ( -3.999999999999997335, -24.17555931017360393, -14.27111468035787745 ) ) ;
#13272 = CIRCLE ( 'NONE', #1464, 10.00000000000000000 ) ;
#13273 = CARTESIAN_POINT ( 'NONE',  ( -4.243569643750005227, -23.82082603165501666, -5.466695036996486401 ) ) ;
#13274 = CARTESIAN_POINT ( 'NONE',  ( -6.774459155162589674, -14.04910063648303264, -1.424143818374616233 ) ) ;
#13275 = PRESENTATION_LAYER_ASSIGNMENT (  '', '', ( #9417 ) ) ;
#13276 = TOROIDAL_SURFACE ( 'NONE', #10605, 9.000000000000003553, 0.9999999999999991118 ) ;
#13277 = LINE ( 'NONE', #7985, #9385 ) ;
#13278 = ADVANCED_FACE ( 'NONE', ( #2425 ), #4065, .T. ) ;
#13279 = CARTESIAN_POINT ( 'NONE',  ( -1.734723475976807094E-15, 43.00000000000000000, -2.500000000000000000 ) ) ;
#13280 = ADVANCED_FACE ( 'NONE', ( #12683 ), #5544, .T. ) ;
#13281 = DIRECTION ( 'NONE',  ( 0.000000000000000000, 0.000000000000000000, 1.000000000000000000 ) ) ;
#13282 = ORIENTED_EDGE ( 'NONE', *, *, #8679, .F. ) ;
#13283 = ORIENTED_EDGE ( 'NONE', *, *, #1672, .F. ) ;
#13284 = DIRECTION ( 'NONE',  ( -1.000000000000000000, -0.000000000000000000, -0.000000000000000000 ) ) ;
#13285 = APPLICATION_CONTEXT ( 'automotive_design' ) ;
#13286 = CARTESIAN_POINT ( 'NONE',  ( -5.577813053751546416E-15, -24.09569370782749331, -3.156949689997003539 ) ) ;
#13287 = CARTESIAN_POINT ( 'NONE',  ( 0.3999999999999975797, 0.000000000000000000, 6.500000000000000000 ) ) ;
#13288 = EDGE_CURVE ( 'NONE', #6366, #17369, #1303, .T. ) ;
#13289 = VERTEX_POINT ( 'NONE', #15401 ) ;
#13290 = CARTESIAN_POINT ( 'NONE',  ( 1.593127413382953383, 30.37819992234354061, -2.091722143975172532 ) ) ;
#13291 = CARTESIAN_POINT ( 'NONE',  ( 4.730628863548789710E-15, -21.98351755778634953, -15.65721693719472185 ) ) ;
#13292 = CARTESIAN_POINT ( 'NONE',  ( 2.211161402132902243, 24.62180007765647716, 2.942372952327172442 ) ) ;
#13293 = PRODUCT ( 'valve seat', 'valve seat', '', ( #3490 ) ) ;
#13294 = EDGE_CURVE ( 'NONE', #14197, #9655, #5560, .T. ) ;
#13295 = DIRECTION ( 'NONE',  ( 0.000000000000000000, 0.4999999999999992784, -0.8660254037844389297 ) ) ;
#13296 = CARTESIAN_POINT ( 'NONE',  ( -2.000000000000005773, -26.77553332299520150, -7.918467616653980024 ) ) ;
#13297 = CARTESIAN_POINT ( 'NONE',  ( 2.121784821875004390, -21.75021530132177006, -13.18828172883567973 ) ) ;
#13298 = EDGE_CURVE ( 'NONE', #6273, #17654, #15933, .T. ) ;
#13299 = TOROIDAL_SURFACE ( 'NONE', #15673, 9.000000000000003553, 0.9999999999999991118 ) ;
#13300 = CIRCLE ( 'NONE', #5611, 2.000000000000001776 ) ;
#13301 = CARTESIAN_POINT ( 'NONE',  ( 4.243569643750003451, -22.22671388484159039, -11.73304717528426622 ) ) ;
#13302 = DIRECTION ( 'NONE',  ( -1.000000000000000000, 0.000000000000000000, 0.000000000000000000 ) ) ;
#13303 = AXIS2_PLACEMENT_3D ( 'NONE', #4331, #14071, #5639 ) ;
#13304 = CARTESIAN_POINT ( 'NONE',  ( -4.000000000000000888, -26.30391020327834539, -13.28439685891468613 ) ) ;
#13305 = CARTESIAN_POINT ( 'NONE',  ( 4.243569643750000786, -27.09437022997710187, -14.41329077045383578 ) ) ;
#13306 = CARTESIAN_POINT ( 'NONE',  ( 2.121784821875004390, -20.94362343770310986, -12.03634916655427922 ) ) ;
#13307 = DIRECTION ( 'NONE',  ( -0.000000000000000000, -1.000000000000000000, -0.000000000000000000 ) ) ;
#13308 = CARTESIAN_POINT ( 'NONE',  ( -1.734723475976807094E-15, 20.99999999999999289, -2.500000000000000000 ) ) ;
#13309 = CARTESIAN_POINT ( 'NONE',  ( -0.7188294034286043521, 27.49680007765648071, 2.395093729190366005 ) ) ;
#13310 = ORIENTED_EDGE ( 'NONE', *, *, #7729, .T. ) ;
#13311 = CARTESIAN_POINT ( 'NONE',  ( -3.518350579753630303, 28.12180007765647716, -1.080741659609802952 ) ) ;
#13312 = CYLINDRICAL_SURFACE ( 'NONE', #8646, 4.000000000000000000 ) ;
#13313 = APPLICATION_PROTOCOL_DEFINITION ( 'draft international standard', 'automotive_design', 1998, #6653 ) ;
#13314 = CARTESIAN_POINT ( 'NONE',  ( -8.000000000000001776, 31.99999999999999289, 2.499999999999998224 ) ) ;
#13315 = CARTESIAN_POINT ( 'NONE',  ( -2.115076519116425580, 19.87819992234354416, -3.012182706137062738 ) ) ;
#13316 = EDGE_LOOP ( 'NONE', ( #2359, #16549, #3223, #9185 ) ) ;
#13317 = CARTESIAN_POINT ( 'NONE',  ( 4.243569643749997233, -24.50911775527627157, -6.449677490143276515 ) ) ;
#13318 = VECTOR ( 'NONE', #1254, 1000.000000000000000 ) ;
#13319 = CARTESIAN_POINT ( 'NONE',  ( -3.673772985318219053, 38.24680007765647360, -2.599342558260952174 ) ) ;
#13320 = CIRCLE ( 'NONE', #1198, 2.999999999999999112 ) ;
#13321 =( BOUNDED_CURVE ( )  B_SPLINE_CURVE ( 2, ( #4529, #8880, #14746, #11749, #1856, #4712, #16137, #7489, #17542 ),
 .UNSPECIFIED., .F., .F. ) 
 B_SPLINE_CURVE_WITH_KNOTS ( ( 3, 2, 2, 2, 3 ),
 ( 0.3706896551724138122, 0.3735632183908045856, 0.3793103448275861878, 0.3850574712643677899, 0.3879310344827586188 ),
 .UNSPECIFIED. ) 
 CURVE ( )  GEOMETRIC_REPRESENTATION_ITEM ( )  RATIONAL_B_SPLINE_CURVE ( ( 0.9330127018922194093, 0.9330127018922200755, 1.000000000000000000, 0.8660254037844387076, 1.000000000000000000, 0.8660254037844387076, 1.000000000000000000, 0.9330127018922194093, 0.9330127018922194093 ) ) 
 REPRESENTATION_ITEM ( '' )  );
#13322 = VERTEX_POINT ( 'NONE', #12590 ) ;
#13323 = DIRECTION ( 'NONE',  ( -0.000000000000000000, -0.000000000000000000, -1.000000000000000000 ) ) ;
#13324 = DIRECTION ( 'NONE',  ( 0.000000000000000000, 0.000000000000000000, 1.000000000000000000 ) ) ;
#13325 = CARTESIAN_POINT ( 'NONE',  ( -4.243569643749997233, -23.72159747208149128, -13.86796219071246306 ) ) ;
#13326 = FACE_OUTER_BOUND ( 'NONE', #1994, .T. ) ;
#13327 = FACE_OUTER_BOUND ( 'NONE', #7393, .T. ) ;
#13328 = CARTESIAN_POINT ( 'NONE',  ( 4.898587196589413815E-16, 2.700915433685006750, 35.11257424290206330 ) ) ;
#13329 = CARTESIAN_POINT ( 'NONE',  ( 2.121784821874994176, -29.88969486959749844, -11.99819291526277532 ) ) ;
#13330 = ORIENTED_EDGE ( 'NONE', *, *, #13177, .F. ) ;
#13331 = CARTESIAN_POINT ( 'NONE',  ( 4.898587196589409870E-16, 4.000000000000007105, -4.000000000000000000 ) ) ;
#13332 = CARTESIAN_POINT ( 'NONE',  ( -2.000000000000005773, -25.80762308735776145, -6.536148542923068128 ) ) ;
#13333 = CIRCLE ( 'NONE', #2694, 0.9999999999999991118 ) ;
#13334 = CARTESIAN_POINT ( 'NONE',  ( 4.898587196589413815E-16, 2.700915433685006750, 35.11257424290206330 ) ) ;
#13335 = VERTEX_POINT ( 'NONE', #18276 ) ;
#13336 = VERTEX_POINT ( 'NONE', #5550 ) ;
#13337 = LINE ( 'NONE', #3335, #16971 ) ;
#13338 = LINE ( 'NONE', #271, #8953 ) ;
#13339 =( LENGTH_UNIT ( ) NAMED_UNIT ( * ) SI_UNIT ( .MILLI., .METRE. ) );
#13340 = CARTESIAN_POINT ( 'NONE',  ( -4.518350579753602325, 29.37819992234355126, 1.405661355842794391 ) ) ;
#13341 = CARTESIAN_POINT ( 'NONE',  ( 4.299564228933482956E-15, -21.02695420434810814, -12.72190984986098172 ) ) ;
#13342 = CARTESIAN_POINT ( 'NONE',  ( 1.989345975306457071, 21.00319992234354771, 1.515154207786300500 ) ) ;
#13343 = ORIENTED_EDGE ( 'NONE', *, *, #5157, .F. ) ;
#13344 = CARTESIAN_POINT ( 'NONE',  ( 1.336863392178479160, 16.24680007765647716, -4.297206761780677731 ) ) ;
#13345 = CARTESIAN_POINT ( 'NONE',  ( -1.999999999999996225, -19.37955217461227875, -9.434865602924197958 ) ) ;
#13346 = ORIENTED_EDGE ( 'NONE', *, *, #13976, .T. ) ;
#13347 = TOROIDAL_SURFACE ( 'NONE', #6827, 9.000000000000003553, 0.9999999999999991118 ) ;
#13348 = CARTESIAN_POINT ( 'NONE',  ( 4.400000000000002132, -26.97786251599087137, -14.24690051095422660 ) ) ;
#13349 = CARTESIAN_POINT ( 'NONE',  ( 3.481649420246369697, 34.12180007765648071, -1.193696214020541824 ) ) ;
#13350 = CARTESIAN_POINT ( 'NONE',  ( -997.9783121635130101, 0.000000000000000000, 0.000000000000000000 ) ) ;
#13351 = CARTESIAN_POINT ( 'NONE',  ( -2.121784821875005722, -22.96375940065866672, -2.106931980473163879 ) ) ;
#13352 = CARTESIAN_POINT ( 'NONE',  ( 4.243569643750003451, -21.48464937031242883, -10.67326921798538386 ) ) ;
#13353 = ADVANCED_FACE ( 'NONE', ( #17156 ), #4430, .F. ) ;
#13354 = EDGE_LOOP ( 'NONE', ( #14770, #13283 ) ) ;
#13355 = CARTESIAN_POINT ( 'NONE',  ( -5.954418220269360518, -10.00000000000000178, 20.87519200589466095 ) ) ;
#13356 = PLANE ( 'NONE',  #3944 ) ;
#13357 = DIRECTION ( 'NONE',  ( 1.000000000000000000, 0.000000000000000000, -0.000000000000000000 ) ) ;
#13358 = CARTESIAN_POINT ( 'NONE',  ( -2.121784821874996396, -23.77207223945918457, -16.07579268495438996 ) ) ;
#13359 = VERTEX_POINT ( 'NONE', #17253 ) ;
#13360 = CARTESIAN_POINT ( 'NONE',  ( -2.115076519116425580, 29.87819992234353350, -3.012182706137062738 ) ) ;
#13361 = CARTESIAN_POINT ( 'NONE',  ( -1.027846397803611866, 15.00319992234354594, -3.346150245485499219 ) ) ;
#13362 = CARTESIAN_POINT ( 'NONE',  ( -4.243569643750000786, -21.02879941556483345, -5.750757902097718421 ) ) ;
#13363 = CARTESIAN_POINT ( 'NONE',  ( 0.05938372350926800214, 24.87180007765647716, 2.628655560595669183 ) ) ;
#13364 = CARTESIAN_POINT ( 'NONE',  ( -1.444289557195956863, 21.50319992234354771, 4.262301884875733471 ) ) ;
#13365 = CARTESIAN_POINT ( 'NONE',  ( -4.243569643750000786, -26.48136041362692339, -13.53782202311997551 ) ) ;
#13366 = CARTESIAN_POINT ( 'NONE',  ( 2.000000000000004441, -23.03610195635016922, -14.65695988526653792 ) ) ;
#13367 = CARTESIAN_POINT ( 'NONE',  ( -2.121784821874996396, -18.60988431229980833, -8.703424286353433459 ) ) ;
#13368 = CARTESIAN_POINT ( 'NONE',  ( 4.481649420246366589, 39.12180007765647360, -1.518615910253458212 ) ) ;
#13369 = EDGE_CURVE ( 'NONE', #894, #2439, #1478, .T. ) ;
#13370 = DIRECTION ( 'NONE',  ( 0.000000000000000000, 0.000000000000000000, -1.000000000000000000 ) ) ;
#13371 = DIRECTION ( 'NONE',  ( 0.000000000000000000, 0.000000000000000000, 1.000000000000000000 ) ) ;
#13372 = FACE_OUTER_BOUND ( 'NONE', #16406, .T. ) ;
#13373 = VERTEX_POINT ( 'NONE', #11656 ) ;
#13374 = EDGE_LOOP ( 'NONE', ( #11560, #9942, #4337, #12863, #7104, #3598, #14429, #3340 ) ) ;
#13375 = CARTESIAN_POINT ( 'NONE',  ( 19.30950000000002120, 0.000000000000000000, 0.000000000000000000 ) ) ;
#13376 = AXIS2_PLACEMENT_3D ( 'NONE', #11397, #14292, #14381 ) ;
#13377 = FACE_OUTER_BOUND ( 'NONE', #7207, .T. ) ;
#13378 = DIRECTION ( 'NONE',  ( 0.000000000000000000, -0.5735764363510413855, -0.8191520442889951292 ) ) ;
#13379 = EDGE_LOOP ( 'NONE', ( #16196, #5698 ) ) ;
#13380 = VECTOR ( 'NONE', #2633, 1000.000000000000000 ) ;
#13381 = CARTESIAN_POINT ( 'NONE',  ( -2.500000000000001332, 32.00319992234354061, -0.05647727720530596601 ) ) ;
#13382 = CARTESIAN_POINT ( 'NONE',  ( -2.121784821875005722, -28.64216612053397526, -10.21653721893421363 ) ) ;
#13383 = CARTESIAN_POINT ( 'NONE',  ( 2.864755990943265829, 19.49680007765648071, 2.011557305968487697 ) ) ;
#13384 = DIRECTION ( 'NONE',  ( -0.000000000000000000, -0.5735764363510414965, -0.8191520442889950182 ) ) ;
#13385 = CARTESIAN_POINT ( 'NONE',  ( -0.8866433558321317188, -10.00000000000235545, -3.510284692361743897 ) ) ;
#13386 = EDGE_CURVE ( 'NONE', #5664, #8124, #4709, .T. ) ;
#13387 = CARTESIAN_POINT ( 'NONE',  ( 4.243569643749996345, -27.86453990792986701, -11.24171694923389531 ) ) ;
#13388 = VECTOR ( 'NONE', #8683, 1000.000000000000000 ) ;
#13389 = CARTESIAN_POINT ( 'NONE',  ( -1.071796769724486786, -21.01542750362927592, -12.70544801520506972 ) ) ;
#13390 = CARTESIAN_POINT ( 'NONE',  ( 4.243569643750003451, -22.74293267755752623, -12.47028401514436347 ) ) ;
#13391 = CARTESIAN_POINT ( 'NONE',  ( -15.00000000000000178, 13.00000000000000178, 24.99999999999999645 ) ) ;
#13392 = AXIS2_PLACEMENT_3D ( 'NONE', #7277, #14534, #14433 ) ;
#13393 = DIRECTION ( 'NONE',  ( 0.000000000000000000, 0.000000000000000000, -1.000000000000000000 ) ) ;
#13394 = CARTESIAN_POINT ( 'NONE',  ( 13.00000000000000178, 48.00000000000000000, 0.000000000000000000 ) ) ;
#13395 = CARTESIAN_POINT ( 'NONE',  ( 4.730628863548789710E-15, -19.40242359420666318, -11.97103273789424449 ) ) ;
#13396 = ORIENTED_EDGE ( 'NONE', *, *, #17754, .F. ) ;
#13397 = DIRECTION ( 'NONE',  ( -0.000000000000000000, -1.000000000000000000, -0.000000000000000000 ) ) ;
#13398 = LINE ( 'NONE', #2202, #5893 ) ;
#13399 = CARTESIAN_POINT ( 'NONE',  ( -0.8262555684461330152, 30.99680007765647716, -2.360188852285403982 ) ) ;
#13400 = EDGE_LOOP ( 'NONE', ( #14370, #3170, #55, #6849 ) ) ;
#13401 = CARTESIAN_POINT ( 'NONE',  ( -3.481649420246370141, 30.37180007765647716, 1.193696214020542268 ) ) ;
#13402 = FACE_OUTER_BOUND ( 'NONE', #16542, .T. ) ;
#13403 = AXIS2_PLACEMENT_3D ( 'NONE', #15783, #17286, #13170 ) ;
#13404 = CONTEXT_DEPENDENT_SHAPE_REPRESENTATION ( #6888, #5155 ) ;
#13405 = AXIS2_PLACEMENT_3D ( 'NONE', #5739, #1573, #11378 ) ;
#13406 = CARTESIAN_POINT ( 'NONE',  ( -1.661723472263481630E-14, -21.09148155414255044, -12.81406445585025544 ) ) ;
#13407 = EDGE_CURVE ( 'NONE', #13486, #1006, #7390, .T. ) ;
#13408 = ORIENTED_EDGE ( 'NONE', *, *, #7443, .T. ) ;
#13409 = CARTESIAN_POINT ( 'NONE',  ( -4.243569643749998122, -20.62428471578586553, -9.444541151551893776 ) ) ;
#13410 = CARTESIAN_POINT ( 'NONE',  ( -0.05938372350928957516, 38.62180007765647360, -4.731580009072201776 ) ) ;
#13411 = EDGE_CURVE ( 'NONE', #14057, #15568, #9306, .T. ) ;
#13412 = ORIENTED_EDGE ( 'NONE', *, *, #3031, .T. ) ;
#13413 = DIRECTION ( 'NONE',  ( 0.000000000000000000, -0.5000000000000012212, -0.8660254037844380415 ) ) ;
#13414 = LINE ( 'NONE', #12383, #7886 ) ;
#13415 = CARTESIAN_POINT ( 'NONE',  ( -1.734723475976807094E-15, 25.39999999999999503, -2.500000000000000000 ) ) ;
#13416 = CIRCLE ( 'NONE', #5426, 0.9999999999999991118 ) ;
#13417 = CARTESIAN_POINT ( 'NONE',  ( 7.402533184386031806, -12.48645682432232284, 8.629691327595670813 ) ) ;
#13418 = COLOUR_RGB ( '',0.8941176470588234615, 0.8941176470588234615, 0.8941176470588234615 ) ;
#13419 = FACE_OUTER_BOUND ( 'NONE', #6464, .T. ) ;
#13420 = CARTESIAN_POINT ( 'NONE',  ( -2.121784821874996396, -17.57744672686793308, -7.228950606633243403 ) ) ;
#13421 = ORIENTED_EDGE ( 'NONE', *, *, #7103, .T. ) ;
#13422 = CYLINDRICAL_SURFACE ( 'NONE', #17216, 8.000000000000000000 ) ;
#13423 = CARTESIAN_POINT ( 'NONE',  ( 4.000000000000000888, -23.14207009859818243, -8.768821215778363154 ) ) ;
#13424 = ORIENTED_EDGE ( 'NONE', *, *, #1627, .F. ) ;
#13425 = EDGE_LOOP ( 'NONE', ( #13602, #11954, #10916, #15181 ) ) ;
#13426 = DIRECTION ( 'NONE',  ( -0.000000000000000000, -0.5000000000000001110, 0.8660254037844385966 ) ) ;
#13427 =( LENGTH_UNIT ( ) NAMED_UNIT ( * ) SI_UNIT ( .MILLI., .METRE. ) );
#13428 = SURFACE_STYLE_FILL_AREA ( #7768 ) ;
#13429 = CARTESIAN_POINT ( 'NONE',  ( -1.444289557195956863, 29.00319992234354771, 4.262301884875733471 ) ) ;
#13430 = CARTESIAN_POINT ( 'NONE',  ( 1.027846397803612311, 38.75319992234354061, 3.346150245485499219 ) ) ;
#13431 = CARTESIAN_POINT ( 'NONE',  ( -1.497042530366522461, 17.37819992234354416, -2.161531897785030409 ) ) ;
#13432 = CIRCLE ( 'NONE', #15806, 0.9999999999999991118 ) ;
#13433 = EDGE_LOOP ( 'NONE', ( #6473, #3904, #5759, #6658 ) ) ;
#13434 = CARTESIAN_POINT ( 'NONE',  ( -1.444289557196047014, 20.99680007765647360, -4.262301884875704161 ) ) ;
#13435 = CARTESIAN_POINT ( 'NONE',  ( 3.999999999999996447, -23.44214610012902966, -5.171056252157234745 ) ) ;
#13436 = ORIENTED_EDGE ( 'NONE', *, *, #11343, .T. ) ;
#13437 = DIRECTION ( 'NONE',  ( -1.000000000000000000, -0.000000000000000000, -0.000000000000000000 ) ) ;
#13438 = CARTESIAN_POINT ( 'NONE',  ( 1.135272562821090458, 34.74680007765648071, 3.311245368580554072 ) ) ;
#13439 = DIRECTION ( 'NONE',  ( -1.000000000000000000, 0.000000000000000000, 4.336808689942021680E-16 ) ) ;
#13440 = CARTESIAN_POINT ( 'NONE',  ( -4.243569643750000786, -20.25447122649092790, -4.644902642307576102 ) ) ;
#13441 = CARTESIAN_POINT ( 'NONE',  ( -5.330712181944245322E-15, -28.36584563134306691, -7.686165607253494514 ) ) ;
#13442 = CARTESIAN_POINT ( 'NONE',  ( -5.577813053751546416E-15, -26.16056887869124381, -6.105897049437384538 ) ) ;
#13443 = VERTEX_POINT ( 'NONE', #11374 ) ;
#13444 = CARTESIAN_POINT ( 'NONE',  ( -0.7594769011887880783, -10.00000000000000178, 23.07585096715833473 ) ) ;
#13445 = DIRECTION ( 'NONE',  ( -0.000000000000000000, -0.5735764363510414965, -0.8191520442889950182 ) ) ;
#13446 = CARTESIAN_POINT ( 'NONE',  ( 0.000000000000000000, 5.000000000000000000, 4.000000000000001776 ) ) ;
#13447 = CARTESIAN_POINT ( 'NONE',  ( 2.121784821874994176, -29.40573975142631014, -11.30703337789393359 ) ) ;
#13448 = VERTEX_POINT ( 'NONE', #14554 ) ;
#13449 = CARTESIAN_POINT ( 'NONE',  ( -0.05938372350920063936, 23.87819992234354416, 3.680117784833935701 ) ) ;
#13450 = EDGE_CURVE ( 'NONE', #12141, #15771, #17063, .T. ) ;
#13451 = DIRECTION ( 'NONE',  ( -3.469446951953613696E-16, -0.000000000000000000, -1.000000000000000000 ) ) ;
#13452 = AXIS2_PLACEMENT_3D ( 'NONE', #17736, #469, #13439 ) ;
#13453 = CARTESIAN_POINT ( 'NONE',  ( 2.121784821874994176, -24.72750694243812219, -4.625824516661818819 ) ) ;
#13454 = CARTESIAN_POINT ( 'NONE',  ( -1.593127413382998459, 23.37180007765648071, -2.091722143975139669 ) ) ;
#13455 = CARTESIAN_POINT ( 'NONE',  ( 4.518350579753602325, 20.62819992234354416, -1.405661355842793725 ) ) ;
#13456 = CARTESIAN_POINT ( 'NONE',  ( -4.243569643749998122, -23.97970686843945742, -14.23658061064251257 ) ) ;
#13457 = CARTESIAN_POINT ( 'NONE',  ( 1.999999999999994449, -29.05549965749059638, -11.17459699270273354 ) ) ;
#13458 = ADVANCED_FACE ( 'NONE', ( #14265 ), #12948, .T. ) ;
#13459 = CARTESIAN_POINT ( 'NONE',  ( -2.121784821875005722, -24.02846066063528596, -3.627482962684610346 ) ) ;
#13460 = EDGE_CURVE ( 'NONE', #15329, #16170, #15344, .T. ) ;
#13461 = CARTESIAN_POINT ( 'NONE',  ( -4.518350579753632523, 38.12180007765647360, -1.405661355842698468 ) ) ;
#13462 = CARTESIAN_POINT ( 'NONE',  ( -2.000000000000005773, -28.32418970114301260, -10.13017813623426733 ) ) ;
#13463 = CARTESIAN_POINT ( 'NONE',  ( 2.000000000000004441, -17.35769523647485713, -6.547354646805487732 ) ) ;
#13464 = DIRECTION ( 'NONE',  ( 0.000000000000000000, 0.8191520442889952403, -0.5735764363510413855 ) ) ;
#13465 = ORIENTED_EDGE ( 'NONE', *, *, #12044, .T. ) ;
#13466 = ORIENTED_EDGE ( 'NONE', *, *, #9208, .F. ) ;
#13467 = CARTESIAN_POINT ( 'NONE',  ( -1.734723475976807094E-15, 23.19999999999999574, -11.50000000000000178 ) ) ;
#13468 = DIRECTION ( 'NONE',  ( 3.469446951953612217E-16, -0.000000000000000000, 1.000000000000000000 ) ) ;
#13469 = CARTESIAN_POINT ( 'NONE',  ( 1.071796769724485232, -29.24635493426803379, -10.51285625394204182 ) ) ;
#13470 = ORIENTED_EDGE ( 'NONE', *, *, #15904, .T. ) ;
#13471 = CARTESIAN_POINT ( 'NONE',  ( -0.7188294034286550893, 30.00319992234354416, -2.395093729190349130 ) ) ;
#13472 = CARTESIAN_POINT ( 'NONE',  ( -4.243569643750000786, -25.41665915365029704, -12.01727104090852905 ) ) ;
#13473 = CARTESIAN_POINT ( 'NONE',  ( 0.05938372350927906274, 22.37180007765648071, 3.680117784833935701 ) ) ;
#13474 = CARTESIAN_POINT ( 'NONE',  ( 8.673617379884035472E-15, 13.00000000000000178, -6.999999999999996447 ) ) ;
#13475 = CARTESIAN_POINT ( 'NONE',  ( -3.999999999999997335, -22.11068413930986054, -11.32216732091749556 ) ) ;
#13476 = CARTESIAN_POINT ( 'NONE',  ( 4.243569643750000786, -25.83608692273200802, -12.61627597329485440 ) ) ;
#13477 = ADVANCED_FACE ( 'NONE', ( #14457 ), #7293, .F. ) ;
#13478 = LINE ( 'NONE', #11993, #9953 ) ;
#13479 = CARTESIAN_POINT ( 'NONE',  ( -3.999999999999997335, -24.43366870653157363, -14.63973310028792518 ) ) ;
#13480 = DIRECTION ( 'NONE',  ( 1.000000000000000000, 0.000000000000000000, 0.000000000000000000 ) ) ;
#13481 = CARTESIAN_POINT ( 'NONE',  ( -4.243569643749997233, -21.88256802303096293, -11.24155594871087338 ) ) ;
#13482 = VERTEX_POINT ( 'NONE', #11558 ) ;
#13483 = DIRECTION ( 'NONE',  ( 0.000000000000000000, 0.000000000000000000, -1.000000000000000000 ) ) ;
#13484 = CARTESIAN_POINT ( 'NONE',  ( 4.000000000000000000, 2.639212418033075380, -1.523750000000004157 ) ) ;
#13485 = CARTESIAN_POINT ( 'NONE',  ( -1.497042530366477164, 32.62180007765647360, 2.161531897785062384 ) ) ;
#13486 = VERTEX_POINT ( 'NONE', #7486 ) ;
#13487 = CARTESIAN_POINT ( 'NONE',  ( -2.211161402132901799, 28.37180007765647716, -2.942372952327172886 ) ) ;
#13488 = PLANE ( 'NONE',  #10727 ) ;
#13489 = PRODUCT_CONTEXT ( 'NONE', #8188, 'mechanical' ) ;
#13490 = DIRECTION ( 'NONE',  ( -0.3258630558627223506, -2.733395053862362198E-16, -0.9454169814551716122 ) ) ;
#13491 = ORIENTED_EDGE ( 'NONE', *, *, #8706, .F. ) ;
#13492 = CARTESIAN_POINT ( 'NONE',  ( -2.121784821874996396, -19.12610310501574418, -9.440661126213528931 ) ) ;
#13493 = CARTESIAN_POINT ( 'NONE',  ( 4.499999999999999112, 39.24680007765647360, -0.05647727720537982360 ) ) ;
#13494 = ORIENTED_EDGE ( 'NONE', *, *, #9321, .F. ) ;
#13495 = VECTOR ( 'NONE', #9664, 1000.000000000000000 ) ;
#13496 = DIRECTION ( 'NONE',  ( 0.000000000000000000, 0.000000000000000000, 1.000000000000000000 ) ) ;
#13497 = AXIS2_PLACEMENT_3D ( 'NONE', #9028, #7630, #2190 ) ;
#13498 = DIRECTION ( 'NONE',  ( -3.469446951953613696E-16, -0.000000000000000000, -1.000000000000000000 ) ) ;
#13499 = CARTESIAN_POINT ( 'NONE',  ( -2.511069452714361550, -24.47646004445711299, -16.25126521642124189 ) ) ;
#13500 = CARTESIAN_POINT ( 'NONE',  ( 9.000000000000005329, 40.79999999999999716, 2.499999999999997335 ) ) ;
#13501 = CARTESIAN_POINT ( 'NONE',  ( 0.000000000000000000, -3.518949890710769246, 4.119968255444916849E-15 ) ) ;
#13502 = CARTESIAN_POINT ( 'NONE',  ( 4.243569643750003451, -18.38733661401680308, -6.249848178824808365 ) ) ;
#13503 = ADVANCED_FACE ( 'NONE', ( #13144 ), #4526, .T. ) ;
#13504 = ORIENTED_EDGE ( 'NONE', *, *, #13752, .F. ) ;
#13505 = LINE ( 'NONE', #17892, #10066 ) ;
#13506 = CARTESIAN_POINT ( 'NONE',  ( -4.000000000000000888, -22.49679660770325285, -7.847275165953248255 ) ) ;
#13507 = CARTESIAN_POINT ( 'NONE',  ( 3.481649420246369697, 34.12180007765648071, -1.193696214020541824 ) ) ;
#13508 = ADVANCED_FACE ( 'NONE', ( #1569 ), #10167, .T. ) ;
#13509 = EDGE_LOOP ( 'NONE', ( #8777, #12, #15510, #2634 ) ) ;
#13510 = ORIENTED_EDGE ( 'NONE', *, *, #8996, .T. ) ;
#13511 = CARTESIAN_POINT ( 'NONE',  ( 0.000000000000000000, 10.00000000000000000, 4.000000000000000000 ) ) ;
#13512 = EDGE_CURVE ( 'NONE', #6584, #17470, #11745, .T. ) ;
#13513 = CARTESIAN_POINT ( 'NONE',  ( -4.481649420246396787, 32.12819992234354771, -1.518615910253363399 ) ) ;
#13514 = CARTESIAN_POINT ( 'NONE',  ( -1.135272562821019626, 39.00319992234354061, 3.311245368580577164 ) ) ;
#13515 = VECTOR ( 'NONE', #15461, 1000.000000000000000 ) ;
#13516 = CARTESIAN_POINT ( 'NONE',  ( -2.518350579753611207, 24.37819992234354416, 0.7558219633769609480 ) ) ;
#13517 = EDGE_LOOP ( 'NONE', ( #17249, #9238, #6768, #17540 ) ) ;
#13518 = ADVANCED_FACE ( 'NONE', ( #5819 ), #15942, .T. ) ;
#13519 = CARTESIAN_POINT ( 'NONE',  ( -3.673772985318219053, 15.74680007765647716, -2.599342558260952174 ) ) ;
#13520 = CARTESIAN_POINT ( 'NONE',  ( -2.000000000000005773, -23.67822056669957576, -3.495046577493408968 ) ) ;
#13521 = VERTEX_POINT ( 'NONE', #6002 ) ;
#13522 = CARTESIAN_POINT ( 'NONE',  ( -8.000000000000003553, 27.59999999999999432, -2.500000000000001776 ) ) ;
#13523 = CARTESIAN_POINT ( 'NONE',  ( -0.05938372350927861171, 36.12180007765648782, -3.680117784833935701 ) ) ;
#13524 = FACE_OUTER_BOUND ( 'NONE', #13146, .T. ) ;
#13525 = CARTESIAN_POINT ( 'NONE',  ( -9.000000000000001776, 36.39999999999999147, 2.499999999999998224 ) ) ;
#13526 = VECTOR ( 'NONE', #16263, 1000.000000000000000 ) ;
#13527 = CARTESIAN_POINT ( 'NONE',  ( -4.243569643749997233, -22.17294109393367307, -11.65625167113217664 ) ) ;
#13528 = PRODUCT_DEFINITION ( 'UNKNOWN', '', #5689, #209 ) ;
#13529 = CARTESIAN_POINT ( 'NONE',  ( 1.342650718860975534, -30.09701863977672431, -12.10727608660696752 ) ) ;
#13530 = ORIENTED_EDGE ( 'NONE', *, *, #9326, .T. ) ;
#13531 = CARTESIAN_POINT ( 'NONE',  ( -3.999999999999997335, -17.98093379758235955, -5.424272602036731783 ) ) ;
#13532 = CARTESIAN_POINT ( 'NONE',  ( 2.864755990943265829, 16.99680007765647716, 2.011557305968487697 ) ) ;
#13533 = CARTESIAN_POINT ( 'NONE',  ( 2.121784821875004390, -23.55698107582754730, -15.76861066834601210 ) ) ;
#13534 = VERTEX_POINT ( 'NONE', #10982 ) ;
#13535 = CARTESIAN_POINT ( 'NONE',  ( 2.115076519116426024, 38.62819992234354771, 3.012182706137062294 ) ) ;
#13536 = FACE_BOUND ( 'NONE', #9622, .T. ) ;
#13537 = CARTESIAN_POINT ( 'NONE',  ( -2.121784821874996396, -17.54518305232318554, -7.182873304141986992 ) ) ;
#13538 = CARTESIAN_POINT ( 'NONE',  ( -1.989345975306426206, 22.74680007765647716, 1.515154207786343799 ) ) ;
#13539 = AXIS2_PLACEMENT_3D ( 'NONE', #11047, #9831, #18217 ) ;
#13540 = CARTESIAN_POINT ( 'NONE',  ( -4.518350579753602325, 16.87819992234354416, 1.405661355842794391 ) ) ;
#13541 = VECTOR ( 'NONE', #14333, 1000.000000000000000 ) ;
#13542 = CARTESIAN_POINT ( 'NONE',  ( 4.000000000000003553, -23.74537698291033294, -13.65675064714112885 ) ) ;
#13543 = EDGE_LOOP ( 'NONE', ( #3677, #4705, #14647, #1554 ) ) ;
#13544 = CARTESIAN_POINT ( 'NONE',  ( 2.121784821875004390, -18.39479314866817461, -8.396242269745057385 ) ) ;
#13545 = CARTESIAN_POINT ( 'NONE',  ( 2.829195390882805583, 39.62180007765647360, 3.793023760679204770 ) ) ;
#13546 = DIRECTION ( 'NONE',  ( -0.000000000000000000, -1.000000000000000000, -0.000000000000000000 ) ) ;
#13547 = CIRCLE ( 'NONE', #7321, 2.000000000000001776 ) ;
#13548 = DIRECTION ( 'NONE',  ( -0.000000000000000000, -1.000000000000000000, -0.000000000000000000 ) ) ;
#13549 = ORIENTED_EDGE ( 'NONE', *, *, #5595, .T. ) ;
#13550 = AXIS2_PLACEMENT_3D ( 'NONE', #2739, #8452, #4116 ) ;
#13551 = VERTEX_POINT ( 'NONE', #10456 ) ;
#13552 = CARTESIAN_POINT ( 'NONE',  ( 2.798362969681366330, 18.99680007765648071, -2.102939460078824929 ) ) ;
#13553 = DIRECTION ( 'NONE',  ( 1.000000000000000000, 0.000000000000000000, -4.336808689942021680E-16 ) ) ;
#13554 = CYLINDRICAL_SURFACE ( 'NONE', #9121, 4.000000000000000000 ) ;
#13555 = ORIENTED_EDGE ( 'NONE', *, *, #13115, .T. ) ;
#13556 = CARTESIAN_POINT ( 'NONE',  ( 0.8262555684460829442, 27.75319992234355126, -2.360188852285421302 ) ) ;
#13557 = DIRECTION ( 'NONE',  ( 0.000000000000000000, 0.000000000000000000, 1.000000000000000000 ) ) ;
#13558 = CARTESIAN_POINT ( 'NONE',  ( -2.121784821874996396, -21.15871460133474713, -12.34353118316265707 ) ) ;
#13559 = CARTESIAN_POINT ( 'NONE',  ( 2.864755990943265829, 26.99680007765648071, 2.011557305968487697 ) ) ;
#13560 = ADVANCED_FACE ( 'NONE', ( #9492 ), #16134, .F. ) ;
#13561 = CARTESIAN_POINT ( 'NONE',  ( 0.000000000000000000, 9.254131787996968228, 30.52396275209373044 ) ) ;
#13562 = CARTESIAN_POINT ( 'NONE',  ( -1.071796769724486564, -27.20453316484195483, -7.596832563813487482 ) ) ;
#13563 = CIRCLE ( 'NONE', #7632, 4.000000000000000888 ) ;
#13564 = CARTESIAN_POINT ( 'NONE',  ( -4.243569643750000786, -25.96514162091098399, -12.80058518325988182 ) ) ;
#13565 = VECTOR ( 'NONE', #2889, 1000.000000000000000 ) ;
#13566 = CARTESIAN_POINT ( 'NONE',  ( 4.074955379826664448, -26.45924826029166965, -14.98212748481132905 ) ) ;
#13567 = CARTESIAN_POINT ( 'NONE',  ( 4.499999999999999112, 19.24680007765647716, -0.05647727720537982360 ) ) ;
#13568 = DIRECTION ( 'NONE',  ( 3.469446951953612217E-16, -0.000000000000000000, 1.000000000000000000 ) ) ;
#13569 = CARTESIAN_POINT ( 'NONE',  ( 2.121784821875004390, -20.68551404134514016, -11.66773074662423149 ) ) ;
#13570 = ORIENTED_EDGE ( 'NONE', *, *, #17545, .F. ) ;
#13571 = CARTESIAN_POINT ( 'NONE',  ( 0.000000000000000000, 5.977523610840987267, 32.81826849749789687 ) ) ;
#13572 = DIRECTION ( 'NONE',  ( -3.469446951953613696E-16, -0.000000000000000000, -1.000000000000000000 ) ) ;
#13573 = CARTESIAN_POINT ( 'NONE',  ( 2.500000000000001332, 26.74680007765648071, -0.05647727720535888202 ) ) ;
#13575 = EDGE_CURVE ( 'NONE', #634, #3783, #14756, .T. ) ;
#13574 = CIRCLE ( 'NONE', #7954, 4.000000000000000888 ) ;
#13576 = AXIS2_PLACEMENT_3D ( 'NONE', #9450, #15123, #3706 ) ;
#13577 = ORIENTED_EDGE ( 'NONE', *, *, #13638, .F. ) ;
#13578 = CARTESIAN_POINT ( 'NONE',  ( 1.027846397803542144, 33.74680007765648071, -3.346150245485522312 ) ) ;
#13579 = CARTESIAN_POINT ( 'NONE',  ( 0.000000000000000000, 36.39999999999999147, 2.500000000000000000 ) ) ;
#13580 = PRODUCT_CONTEXT ( 'NONE', #5944, 'mechanical' ) ;
#13581 = DIRECTION ( 'NONE',  ( 0.000000000000000000, 0.000000000000000000, -1.000000000000000000 ) ) ;
#13582 = MECHANICAL_DESIGN_GEOMETRIC_PRESENTATION_REPRESENTATION (  '', ( #1322 ), #10883 ) ;
#13583 =( BOUNDED_CURVE ( )  B_SPLINE_CURVE ( 2, ( #12202, #9331, #5068, #10909, #9420, #15279, #3954, #4980, #8031 ),
 .UNSPECIFIED., .F., .T. ) 
 B_SPLINE_CURVE_WITH_KNOTS ( ( 3, 2, 2, 2, 3 ),
 ( 0.8362068965517241992, 0.8390804597701149170, 0.8448275862068965747, 0.8505747126436781214, 0.8534482758620689502 ),
 .UNSPECIFIED. ) 
 CURVE ( )  GEOMETRIC_REPRESENTATION_ITEM ( )  RATIONAL_B_SPLINE_CURVE ( ( 0.9330127018922194093, 0.9330127018922206306, 1.000000000000000000, 0.8660254037844387076, 1.000000000000000000, 0.8660254037844387076, 1.000000000000000000, 0.9330127018922194093, 0.9330127018922194093 ) ) 
 REPRESENTATION_ITEM ( '' )  );
#13584 = ORIENTED_EDGE ( 'NONE', *, *, #7337, .F. ) ;
#13585 = CARTESIAN_POINT ( 'NONE',  ( -5.330712181944246111E-15, -26.81718925319525937, -5.474455087673208986 ) ) ;
#13586 = CARTESIAN_POINT ( 'NONE',  ( -2.115076519116362519, 25.12180007765647360, 3.012182706137107147 ) ) ;
#13587 = AXIS2_PLACEMENT_3D ( 'NONE', #13308, #11722, #6260 ) ;
#13588 = VERTEX_POINT ( 'NONE', #17873 ) ;
#13589 = AXIS2_PLACEMENT_3D ( 'NONE', #15650, #1840, #4516 ) ;
#13590 = CARTESIAN_POINT ( 'NONE',  ( -9.000000000000003553, 27.59999999999999432, -2.500000000000001776 ) ) ;
#13591 = AXIS2_PLACEMENT_3D ( 'NONE', #17553, #8992, #17456 ) ;
#13592 = CYLINDRICAL_SURFACE ( 'NONE', #6488, 2.149999999999995470 ) ;
#13593 = CARTESIAN_POINT ( 'NONE',  ( 8.399999999999998579, 0.000000000000000000, 0.000000000000000000 ) ) ;
#13594 = CARTESIAN_POINT ( 'NONE',  ( 4.551717183842061587, -10.00000000000000178, -2.180355508048899882 ) ) ;
#13595 = CARTESIAN_POINT ( 'NONE',  ( 1.071796769724494780, -27.95580795247818173, -8.669764154291803138 ) ) ;
#13596 = CARTESIAN_POINT ( 'NONE',  ( -4.243569643750005227, -28.95075028426964181, -12.79298613310618471 ) ) ;
#13597 = ORIENTED_EDGE ( 'NONE', *, *, #7156, .T. ) ;
#13598 = CARTESIAN_POINT ( 'NONE',  ( -31.74999999999995737, 7.960204194457795477E-16, -6.500000000000000000 ) ) ;
#13599 = CARTESIAN_POINT ( 'NONE',  ( 3.999999999999996447, -25.57154862078722246, -8.212158217586894793 ) ) ;
#13600 = AXIS2_PLACEMENT_3D ( 'NONE', #16381, #3303, #16108 ) ;
#13601 = CARTESIAN_POINT ( 'NONE',  ( 2.864755990943265829, 29.49680007765647716, 2.011557305968487697 ) ) ;
#13602 = ORIENTED_EDGE ( 'NONE', *, *, #9430, .F. ) ;
#13603 = ORIENTED_EDGE ( 'NONE', *, *, #2647, .T. ) ;
#13604 = CARTESIAN_POINT ( 'NONE',  ( 4.000000000000003553, -20.45448218005117624, -8.956865794039783779 ) ) ;
#13605 = AXIS2_PLACEMENT_3D ( 'NONE', #10067, #5995, #10255 ) ;
#13606 = CARTESIAN_POINT ( 'NONE',  ( -3.607379964056363075, 32.25319992234354061, -2.690724712371229899 ) ) ;
#13607 = CARTESIAN_POINT ( 'NONE',  ( -2.798362969681409851, 34.75319992234354771, -2.102939460078765421 ) ) ;
#13608 = CARTESIAN_POINT ( 'NONE',  ( -0.7188294034286550893, 25.00319992234354771, -2.395093729190349130 ) ) ;
#13609 = ORIENTED_EDGE ( 'NONE', *, *, #10968, .F. ) ;
#13610 = CARTESIAN_POINT ( 'NONE',  ( -0.05938372350928957516, 28.62180007765647005, -4.731580009072201776 ) ) ;
#13611 = CARTESIAN_POINT ( 'NONE',  ( 4.000000000000003553, -19.35751724482486580, -7.390237508330316452 ) ) ;
#13612 = ORIENTED_EDGE ( 'NONE', *, *, #14142, .F. ) ;
#13613 = EDGE_CURVE ( 'NONE', #15568, #14065, #12275, .T. ) ;
#13614 = CARTESIAN_POINT ( 'NONE',  ( -3.999999999999997335, -19.78769957208813679, -8.004601541547065935 ) ) ;
#13615 = EDGE_CURVE ( 'NONE', #9512, #11364, #14136, .T. ) ;
#13616 = CARTESIAN_POINT ( 'NONE',  ( 1.027846397803542144, 36.24680007765648071, -3.346150245485522312 ) ) ;
#13617 = CARTESIAN_POINT ( 'NONE',  ( 4.299564228933482956E-15, -17.41342265533655009, -7.561251970840314307 ) ) ;
#13618 = CONICAL_SURFACE ( 'NONE', #15117, 1.610000000000000098, 0.7853981633974469467 ) ;
#13619 = DIRECTION ( 'NONE',  ( 0.000000000000000000, 0.000000000000000000, 1.000000000000000000 ) ) ;
#13620 = CARTESIAN_POINT ( 'NONE',  ( -2.121784821874996396, -20.93286887952152497, -12.02099006572386486 ) ) ;
#13621 = EDGE_CURVE ( 'NONE', #17766, #5913, #3491, .T. ) ;
#13622 = CARTESIAN_POINT ( 'NONE',  ( -4.000000000000004441, -24.81872954737152170, -7.137021158450828295 ) ) ;
#13623 = ORIENTED_EDGE ( 'NONE', *, *, #4731, .F. ) ;
#13624 = CYLINDRICAL_SURFACE ( 'NONE', #16357, 4.000000000000000000 ) ;
#13625 = DIRECTION ( 'NONE',  ( -0.000000000000000000, -1.000000000000000000, -0.000000000000000000 ) ) ;
#13626 = CARTESIAN_POINT ( 'NONE',  ( -4.000000000000004441, -24.56062015101355911, -6.768402738520781448 ) ) ;
#13627 = CARTESIAN_POINT ( 'NONE',  ( -1.071796769724496334, -25.97851353284654152, -5.845895070152532291 ) ) ;
#13628 = VERTEX_POINT ( 'NONE', #12455 ) ;
#13629 = CARTESIAN_POINT ( 'NONE',  ( -2.798362969681409851, 32.25319992234354771, -2.102939460078765421 ) ) ;
#13630 = CARTESIAN_POINT ( 'NONE',  ( 2.211161402132839182, 15.37819992234354594, -2.942372952327217739 ) ) ;
#13631 = CARTESIAN_POINT ( 'NONE',  ( -4.243569643750000786, -20.25447122649092790, -4.644902642307576102 ) ) ;
#13632 = CARTESIAN_POINT ( 'NONE',  ( -1.593127413382998459, 30.87180007765647716, -2.091722143975139669 ) ) ;
#13633 = AXIS2_PLACEMENT_3D ( 'NONE', #13279, #7713, #864 ) ;
#13634 = CARTESIAN_POINT ( 'NONE',  ( 3.673772985318163098, 28.00319992234354771, -2.599342558261029001 ) ) ;
#13635 = CARTESIAN_POINT ( 'NONE',  ( 3.999999999999996447, -27.31378704549856096, -10.70033255110795167 ) ) ;
#13636 = ORIENTED_EDGE ( 'NONE', *, *, #9701, .F. ) ;
#13637 = CARTESIAN_POINT ( 'NONE',  ( -4.243569643750000786, -20.02862550467770220, -4.322361524868783889 ) ) ;
#13638 = EDGE_CURVE ( 'NONE', #2662, #10239, #2310, .T. ) ;
#13639 = CARTESIAN_POINT ( 'NONE',  ( -4.499999999999999112, 40.49680007765648071, 0.05647727720537927543 ) ) ;
#13640 = CARTESIAN_POINT ( 'NONE',  ( -1.071796769724491671, -22.30597448541912087, -14.54854011485530840 ) ) ;
#13641 = AXIS2_PLACEMENT_3D ( 'NONE', #7575, #3422, #17000 ) ;
#13642 = CARTESIAN_POINT ( 'NONE',  ( 1.999999999999994449, -27.24873388298481558, -8.594268053192397616 ) ) ;
#13643 = DIRECTION ( 'NONE',  ( -3.469446951953613696E-16, -0.000000000000000000, -1.000000000000000000 ) ) ;
#13644 = ORIENTED_EDGE ( 'NONE', *, *, #12780, .T. ) ;
#13645 = VERTEX_POINT ( 'NONE', #8195 ) ;
#13646 = FACE_OUTER_BOUND ( 'NONE', #2966, .T. ) ;
#13647 = FACE_OUTER_BOUND ( 'NONE', #343, .T. ) ;
#13648 = CARTESIAN_POINT ( 'NONE',  ( 7.491798610157291982, -13.11847650086634509, 4.256480280831525853 ) ) ;
#13649 = EDGE_LOOP ( 'NONE', ( #567, #14230, #12305, #17334 ) ) ;
#13650 = CARTESIAN_POINT ( 'NONE',  ( -2.518350579753611207, 39.37819992234354771, 0.7558219633769609480 ) ) ;
#13651 = CARTESIAN_POINT ( 'NONE',  ( -5.330712181944245322E-15, -28.33358195679831937, -7.640088304762238103 ) ) ;
#13652 = CARTESIAN_POINT ( 'NONE',  ( 2.211161402132902243, 29.62180007765648071, 2.942372952327172442 ) ) ;
#13653 = CARTESIAN_POINT ( 'NONE',  ( 1.027846397803612311, 16.25319992234354416, 3.346150245485499219 ) ) ;
#13654 = ADVANCED_FACE ( 'NONE', ( #3937 ), #5142, .T. ) ;
#13655 = DIRECTION ( 'NONE',  ( 0.000000000000000000, 0.000000000000000000, 1.000000000000000000 ) ) ;
#13656 = CARTESIAN_POINT ( 'NONE',  ( -2.343145750507620750, 4.000000000000007994, -4.000000000000000888 ) ) ;
#13657 = AXIS2_PLACEMENT_3D ( 'NONE', #9314, #13397, #4958 ) ;
#13658 = CARTESIAN_POINT ( 'NONE',  ( -2.121784821874996396, -21.96530646495340378, -13.49546374544405403 ) ) ;
#13659 = LINE ( 'NONE', #13391, #16206 ) ;
#13660 = CARTESIAN_POINT ( 'NONE',  ( 4.518350579753633411, 26.87180007765647716, 1.405661355842698468 ) ) ;
#13661 = DIRECTION ( 'NONE',  ( 0.000000000000000000, 0.000000000000000000, -1.000000000000000000 ) ) ;
#13662 = CARTESIAN_POINT ( 'NONE',  ( 4.898587196589413815E-16, 2.700915433685006750, 35.11257424290206330 ) ) ;
#13663 = CARTESIAN_POINT ( 'NONE',  ( 2.121784821874994176, -25.50183513151203130, -5.731679776451962915 ) ) ;
#13664 = CARTESIAN_POINT ( 'NONE',  ( -3.999999999999997335, -20.11033631824054524, -8.465374567466390943 ) ) ;
#13666 = CARTESIAN_POINT ( 'NONE',  ( -8.500000000000010658, 14.99364916731036956, 20.49999999999998934 ) ) ;
#13665 =( GEOMETRIC_REPRESENTATION_CONTEXT ( 3 ) GLOBAL_UNCERTAINTY_ASSIGNED_CONTEXT ( ( #16807 ) ) GLOBAL_UNIT_ASSIGNED_CONTEXT ( ( #1483, #16981, #4258 ) ) REPRESENTATION_CONTEXT ( 'NONE', 'WORKASPACE' ) );
#13667 = CARTESIAN_POINT ( 'NONE',  ( -2.055738996568313048, 38.24680007765647360, -1.423772053676023441 ) ) ;
#13668 = DIRECTION ( 'NONE',  ( 0.000000000000000000, 0.000000000000000000, 1.000000000000000000 ) ) ;
#13669 = CARTESIAN_POINT ( 'NONE',  ( -1.027846397803541700, 27.49680007765648071, 3.346150245485522312 ) ) ;
#13670 = CARTESIAN_POINT ( 'NONE',  ( 2.021687836487040535, 0.000000000000000000, 2.168404344971008868E-16 ) ) ;
#13671 = CARTESIAN_POINT ( 'NONE',  ( -4.000000000000002665, 15.00000000000001066, -0.2096920304738193463 ) ) ;
#13672 = AXIS2_PLACEMENT_3D ( 'NONE', #3348, #752, #8994 ) ;
#13673 = ORIENTED_EDGE ( 'NONE', *, *, #8265, .T. ) ;
#13674 = CIRCLE ( 'NONE', #14883, 0.9999999999999991118 ) ;
#13675 = CARTESIAN_POINT ( 'NONE',  ( -2.121784821875005722, -24.28657005699325921, -3.996101382614658970 ) ) ;
#13676 = EDGE_CURVE ( 'NONE', #12007, #15972, #15076, .T. ) ;
#13677 = CARTESIAN_POINT ( 'NONE',  ( 3.481649420246369697, 24.12180007765648071, -1.193696214020541824 ) ) ;
#13678 = AXIS2_PLACEMENT_3D ( 'NONE', #11137, #16823, #5120 ) ;
#13679 = ORIENTED_EDGE ( 'NONE', *, *, #12711, .F. ) ;
#13680 = ADVANCED_FACE ( 'NONE', ( #2381 ), #836, .T. ) ;
#13681 = VERTEX_POINT ( 'NONE', #3383 ) ;
#13682 = CARTESIAN_POINT ( 'NONE',  ( 4.000000000000003553, -19.87373603754079809, -8.127474348190411035 ) ) ;
#13683 = EDGE_CURVE ( 'NONE', #11829, #17908, #14742, .T. ) ;
#13684 = FACE_OUTER_BOUND ( 'NONE', #17166, .T. ) ;
#13685 = CARTESIAN_POINT ( 'NONE',  ( 2.658838382460517735, -24.55987625702158539, -16.27480033055179476 ) ) ;
#13686 = CARTESIAN_POINT ( 'NONE',  ( 7.638598542356191956, -10.30911785226841282, 7.201745306969625560 ) ) ;
#13687 = EDGE_CURVE ( 'NONE', #17470, #1591, #3637, .T. ) ;
#13688 = DIRECTION ( 'NONE',  ( -0.000000000000000000, -1.000000000000000000, -0.000000000000000000 ) ) ;
#13689 = CARTESIAN_POINT ( 'NONE',  ( -4.243569643750000786, -25.67476855000827030, -12.38588946083857856 ) ) ;
#13690 = ORIENTED_EDGE ( 'NONE', *, *, #5542, .F. ) ;
#13691 = CARTESIAN_POINT ( 'NONE',  ( -1.734723475976807094E-15, 36.39999999999999147, -2.500000000000000000 ) ) ;
#13692 = VECTOR ( 'NONE', #6634, 1000.000000000000000 ) ;
#13693 = CARTESIAN_POINT ( 'NONE',  ( 2.000000000000004441, -19.22898836077508022, -9.219838192305099156 ) ) ;
#13694 = AXIS2_PLACEMENT_3D ( 'NONE', #7673, #6198, #8881 ) ;
#13695 = CARTESIAN_POINT ( 'NONE',  ( -3.518350579753630747, 35.62180007765648782, -1.080741659609802729 ) ) ;
#13696 = ORIENTED_EDGE ( 'NONE', *, *, #2090, .F. ) ;
#13697 = VERTEX_POINT ( 'NONE', #3331 ) ;
#13698 =( BOUNDED_CURVE ( )  B_SPLINE_CURVE ( 2, ( #9852, #1069, #15261, #2557, #8189, #9668, #10304, #12998, #11413 ),
 .UNSPECIFIED., .F., .T. ) 
 B_SPLINE_CURVE_WITH_KNOTS ( ( 3, 2, 2, 2, 3 ),
 ( 0.8362068965517241992, 0.8390804597701149170, 0.8448275862068965747, 0.8505747126436781214, 0.8534482758620689502 ),
 .UNSPECIFIED. ) 
 CURVE ( )  GEOMETRIC_REPRESENTATION_ITEM ( )  RATIONAL_B_SPLINE_CURVE ( ( 0.9330127018922194093, 0.9330127018922206306, 1.000000000000000000, 0.8660254037844387076, 1.000000000000000000, 0.8660254037844387076, 1.000000000000000000, 0.9330127018922194093, 0.9330127018922194093 ) ) 
 REPRESENTATION_ITEM ( '' )  );
#13699 = CARTESIAN_POINT ( 'NONE',  ( 3.999999999999996447, -27.37831439529299615, -10.79248715709722717 ) ) ;
#13700 =( LENGTH_UNIT ( ) NAMED_UNIT ( * ) SI_UNIT ( .MILLI., .METRE. ) );
#13701 = CARTESIAN_POINT ( 'NONE',  ( -4.518350579753602325, 36.87819992234354061, 1.405661355842794391 ) ) ;
#13702 = LINE ( 'NONE', #16598, #9562 ) ;
#13703 = CARTESIAN_POINT ( 'NONE',  ( 2.481649420246391902, 30.87819992234354416, 0.8687765177875720335 ) ) ;
#13704 = EDGE_LOOP ( 'NONE', ( #16479, #9050, #1534, #17871 ) ) ;
#13705 = CARTESIAN_POINT ( 'NONE',  ( 3.673772985318219053, 29.49680007765647360, 2.599342558260951730 ) ) ;
#13706 = CARTESIAN_POINT ( 'NONE',  ( 2.000000000000004441, -18.13202342554876267, -7.653209906595630940 ) ) ;
#13707 = ORIENTED_EDGE ( 'NONE', *, *, #17076, .F. ) ;
#13708 = CIRCLE ( 'NONE', #1881, 0.9999999999999991118 ) ;
#13709 = CARTESIAN_POINT ( 'NONE',  ( 4.000000000000000000, -3.518949890710769246, 4.119968255444916849E-15 ) ) ;
#13710 = TOROIDAL_SURFACE ( 'NONE', #12815, 9.000000000000001776, 0.9999999999999991118 ) ;
#13711 = CARTESIAN_POINT ( 'NONE',  ( 2.211161402132902243, 39.62180007765646650, 2.942372952327172442 ) ) ;
#13712 = LINE ( 'NONE', #6664, #16178 ) ;
#13713 = CARTESIAN_POINT ( 'NONE',  ( -5.330712181944246111E-15, -24.72005040778675777, -2.479430425741570243 ) ) ;
#13714 = CARTESIAN_POINT ( 'NONE',  ( 4.730628863548789710E-15, -20.46712485418328242, -13.49158372010569273 ) ) ;
#13715 = CARTESIAN_POINT ( 'NONE',  ( -1.734723475976807094E-15, 20.99999999999999289, -11.50000000000000178 ) ) ;
#13716 = ORIENTED_EDGE ( 'NONE', *, *, #6896, .F. ) ;
#13717 = DIRECTION ( 'NONE',  ( 0.000000000000000000, 0.000000000000000000, 1.000000000000000000 ) ) ;
#13718 = CARTESIAN_POINT ( 'NONE',  ( 3.500000000000000444, 16.74680007765647716, -0.05647727720536935281 ) ) ;
#13719 = AXIS2_PLACEMENT_3D ( 'NONE', #14818, #3406, #10438 ) ;
#13720 =( NAMED_UNIT ( * ) PLANE_ANGLE_UNIT ( ) SI_UNIT ( $, .RADIAN. ) );
#13721 = VERTEX_POINT ( 'NONE', #7577 ) ;
#13722 = CARTESIAN_POINT ( 'NONE',  ( 3.500000000000000444, 35.75319992234354771, 0.05647727720529520379 ) ) ;
#13723 = CARTESIAN_POINT ( 'NONE',  ( -3.518350579753606322, 19.37819992234354416, 1.080741659609877781 ) ) ;
#13724 = CARTESIAN_POINT ( 'NONE',  ( -4.243569643750000786, -19.73825243377498850, -3.907665802447479297 ) ) ;
#13725 = CARTESIAN_POINT ( 'NONE',  ( -0.05938372350926768989, 33.62180007765647360, -2.628655560595669183 ) ) ;
#13726 = ADVANCED_FACE ( 'NONE', ( #8976 ), #1075, .T. ) ;
#13727 = CARTESIAN_POINT ( 'NONE',  ( -4.499999999999999112, 24.50319992234354771, -0.05647727720528529505 ) ) ;
#13728 =( BOUNDED_CURVE ( )  B_SPLINE_CURVE ( 2, ( #16751, #2380, #8012, #13664, #4025, #9672, #1259, #12550, #18237 ),
 .UNSPECIFIED., .F., .T. ) 
 B_SPLINE_CURVE_WITH_KNOTS ( ( 3, 2, 2, 2, 3 ),
 ( 0.6637931034482759118, 0.6666666666666666297, 0.6724137931034482873, 0.6781609195402298340, 0.6810344827586206629 ),
 .UNSPECIFIED. ) 
 CURVE ( )  GEOMETRIC_REPRESENTATION_ITEM ( )  RATIONAL_B_SPLINE_CURVE ( ( 0.9330127018922194093, 0.9330127018922206306, 1.000000000000000000, 0.8660254037844387076, 1.000000000000000000, 0.8660254037844387076, 1.000000000000000000, 0.9330127018922194093, 0.9330127018922194093 ) ) 
 REPRESENTATION_ITEM ( '' )  );
#13729 = CARTESIAN_POINT ( 'NONE',  ( -3.999999999999997335, -23.65934051745766808, -13.53387784049778197 ) ) ;
#13730 = ORIENTED_EDGE ( 'NONE', *, *, #8407, .F. ) ;
#13731 = CARTESIAN_POINT ( 'NONE',  ( 2.121784821874994176, -23.46922363519303190, -2.828809719502837439 ) ) ;
#13732 = CARTESIAN_POINT ( 'NONE',  ( 3.518350579753631191, 16.87180007765648071, 1.080741659609802285 ) ) ;
#13733 = CARTESIAN_POINT ( 'NONE',  ( -4.000000000000000888, -24.30356238220903364, -10.42760410546358152 ) ) ;
#13734 = AXIS2_PLACEMENT_3D ( 'NONE', #12264, #15256, #10970 ) ;
#13735 = CARTESIAN_POINT ( 'NONE',  ( 2.121784821875004390, -20.68551404134514016, -11.66773074662423149 ) ) ;
#13736 = AXIS2_PLACEMENT_3D ( 'NONE', #4768, #4492, #10420 ) ;
#13737 = LINE ( 'NONE', #77, #11447 ) ;
#13738 = CARTESIAN_POINT ( 'NONE',  ( -1.734723475976807094E-15, 34.19999999999999574, -11.50000000000000178 ) ) ;
#13739 = FACE_OUTER_BOUND ( 'NONE', #15537, .T. ) ;
#13740 = EDGE_LOOP ( 'NONE', ( #13679, #10555, #10688, #10611, #17647, #12128 ) ) ;
#13741 = VERTEX_POINT ( 'NONE', #18057 ) ;
#13742 = DIRECTION ( 'NONE',  ( 1.000000000000000000, 0.000000000000000000, -4.336808689942021680E-16 ) ) ;
#13743 = CARTESIAN_POINT ( 'NONE',  ( 0.000000000000000000, 5.000000000000000000, 0.000000000000000000 ) ) ;
#13744 = EDGE_CURVE ( 'NONE', #904, #12007, #17119, .T. ) ;
#13745 = CYLINDRICAL_SURFACE ( 'NONE', #3316, 4.000000000000000000 ) ;
#13746 = CARTESIAN_POINT ( 'NONE',  ( 4.000000000000003553, -22.19672060476252184, -11.44504012756083888 ) ) ;
#13747 = EDGE_LOOP ( 'NONE', ( #16942, #14541, #11734, #10223 ) ) ;
#13748 = CARTESIAN_POINT ( 'NONE',  ( 1.989345975306457071, 38.50319992234354771, 1.515154207786300500 ) ) ;
#13749 = EDGE_CURVE ( 'NONE', #17274, #11085, #13847, .T. ) ;
#13750 = CARTESIAN_POINT ( 'NONE',  ( -2.121784821875005722, -27.60972853510210001, -8.742063539214022683 ) ) ;
#13751 = CARTESIAN_POINT ( 'NONE',  ( -1.027846397803541700, 32.49680007765648071, 3.346150245485522312 ) ) ;
#13752 = EDGE_CURVE ( 'NONE', #6687, #4578, #5847, .T. ) ;
#13753 = CARTESIAN_POINT ( 'NONE',  ( 2.115076519116426024, 28.62819992234353705, 3.012182706137062294 ) ) ;
#13754 = DIRECTION ( 'NONE',  ( 1.000000000000000000, 0.000000000000000000, -4.336808689942021680E-16 ) ) ;
#13755 = DIRECTION ( 'NONE',  ( -3.469446951953613696E-16, -0.000000000000000000, -1.000000000000000000 ) ) ;
#13756 = CARTESIAN_POINT ( 'NONE',  ( -4.243569643749997233, -22.43105049029164277, -12.02487009106222615 ) ) ;
#13757 = FACE_BOUND ( 'NONE', #17327, .T. ) ;
#13758 = CARTESIAN_POINT ( 'NONE',  ( 2.829195390882805583, 22.12180007765647716, 3.793023760679204770 ) ) ;
#13759 = DIRECTION ( 'NONE',  ( 0.000000000000000000, 0.000000000000000000, -1.000000000000000000 ) ) ;
#13760 = CARTESIAN_POINT ( 'NONE',  ( 0.000000000000000000, 9.254131787996968228, 30.52396275209373044 ) ) ;
#13761 = CARTESIAN_POINT ( 'NONE',  ( 2.121784821874994176, -24.46939754608015605, -4.257206096731771083 ) ) ;
#13762 = FACE_OUTER_BOUND ( 'NONE', #12568, .T. ) ;
#13763 = CARTESIAN_POINT ( 'NONE',  ( 1.071796769724500109, -21.87733644393529531, -13.93638155029631420 ) ) ;
#13764 = CARTESIAN_POINT ( 'NONE',  ( -2.500000000000001332, 40.49680007765648071, 0.05647727720535858364 ) ) ;
#13765 = CARTESIAN_POINT ( 'NONE',  ( -9.184850993605147944E-16, 46.00000000000000000, -10.50000000000000000 ) ) ;
#13766 = CARTESIAN_POINT ( 'NONE',  ( -1.135272562821090014, 38.49680007765647360, -3.311245368580554072 ) ) ;
#13767 = DIRECTION ( 'NONE',  ( 0.000000000000000000, 0.000000000000000000, -1.000000000000000000 ) ) ;
#13768 = CONTEXT_DEPENDENT_SHAPE_REPRESENTATION ( #11038, #8248 ) ;
#13769 = CYLINDRICAL_SURFACE ( 'NONE', #4845, 2.149999999999995470 ) ;
#13770 = ORIENTED_EDGE ( 'NONE', *, *, #6706, .T. ) ;
#13771 = CARTESIAN_POINT ( 'NONE',  ( -2.121784821875005722, -25.06089824606716476, -5.101956642404802622 ) ) ;
#13772 = ADVANCED_FACE ( 'NONE', ( #18328 ), #1614, .F. ) ;
#13773 = CARTESIAN_POINT ( 'NONE',  ( 0.05938372350927906274, 27.37180007765647716, 3.680117784833935701 ) ) ;
#13774 = ORIENTED_EDGE ( 'NONE', *, *, #16926, .F. ) ;
#13775 = MANIFOLD_SOLID_BREP ( 'LPattern6[8]', #9404 ) ;
#13776 = CARTESIAN_POINT ( 'NONE',  ( 4.000000000000000888, -21.78699576701389873, -6.833574510138848090 ) ) ;
#13777 = CARTESIAN_POINT ( 'NONE',  ( -2.121784821875005722, -29.67460370596585406, -11.69101089865440457 ) ) ;
#13778 = CARTESIAN_POINT ( 'NONE',  ( -3.291771655530798757, -28.93493258167780269, -13.02337503524261386 ) ) ;
#13779 = DIRECTION ( 'NONE',  ( -1.000000000000000000, 0.000000000000000000, 0.000000000000000000 ) ) ;
#13780 = LINE ( 'NONE', #13501, #17106 ) ;
#13781 = CARTESIAN_POINT ( 'NONE',  ( 4.243569643750003451, -23.51726086663143533, -13.57613927493450667 ) ) ;
#13782 = ORIENTED_EDGE ( 'NONE', *, *, #726, .F. ) ;
#13783 = CARTESIAN_POINT ( 'NONE',  ( 9.000000000000005329, 16.59999999999999787, 2.499999999999997335 ) ) ;
#13784 = CARTESIAN_POINT ( 'NONE',  ( -1.999999999999996225, -18.41164193897483869, -8.052546529193282510 ) ) ;
#13785 = CARTESIAN_POINT ( 'NONE',  ( -3.481649420246369697, 40.37180007765648071, 1.193696214020542490 ) ) ;
#13786 = ORIENTED_EDGE ( 'NONE', *, *, #14211, .T. ) ;
#13787 = ORIENTED_EDGE ( 'NONE', *, *, #870, .T. ) ;
#13788 = CARTESIAN_POINT ( 'NONE',  ( 3.061616997868382648E-16, 5.000000000000000000, 2.499999999999999556 ) ) ;
#13789 = EDGE_CURVE ( 'NONE', #16110, #15565, #15531, .T. ) ;
#13790 = CARTESIAN_POINT ( 'NONE',  ( 3.673772985318163098, 38.00319992234354061, -2.599342558261029001 ) ) ;
#13791 = UNCERTAINTY_MEASURE_WITH_UNIT (LENGTH_MEASURE( 1.000000000000000082E-05 ), #15992, 'distance_accuracy_value', 'NONE');
#13792 = CARTESIAN_POINT ( 'NONE',  ( -4.000000000000004441, -22.23763558379183181, -3.450836959150351824 ) ) ;
#13793 = CARTESIAN_POINT ( 'NONE',  ( -1.989345975306457071, 24.75319992234354416, -1.515154207786300944 ) ) ;
#13794 = CIRCLE ( 'NONE', #15001, 8.000000000000001776 ) ;
#13795 = EDGE_CURVE ( 'NONE', #9873, #8773, #13547, .T. ) ;
#13796 = ORIENTED_EDGE ( 'NONE', *, *, #5017, .F. ) ;
#13797 = CARTESIAN_POINT ( 'NONE',  ( -4.243569643750004339, -27.69246697702454441, -10.99597133594720333 ) ) ;
#13798 = CARTESIAN_POINT ( 'NONE',  ( -3.607379964056306676, 22.74680007765647716, 2.690724712371306282 ) ) ;
#13799 = CARTESIAN_POINT ( 'NONE',  ( 1.999999999999994449, -24.15142112668919339, -4.170847014031824784 ) ) ;
#13800 = ORIENTED_EDGE ( 'NONE', *, *, #4861, .F. ) ;
#13801 = DIRECTION ( 'NONE',  ( -0.000000000000000000, -0.5735764363510414965, -0.8191520442889950182 ) ) ;
#13802 = DIRECTION ( 'NONE',  ( 0.000000000000000000, 0.000000000000000000, -1.000000000000000000 ) ) ;
#13803 = DIRECTION ( 'NONE',  ( 0.000000000000000000, 0.000000000000000000, 1.000000000000000000 ) ) ;
#13804 = DIRECTION ( 'NONE',  ( 0.000000000000000000, 0.000000000000000000, 1.000000000000000000 ) ) ;
#13805 =( BOUNDED_CURVE ( )  B_SPLINE_CURVE ( 2, ( #4125, #5511, #2746, #7323, #11157, #10100, #3268, #13078, #3080 ),
 .UNSPECIFIED., .F., .T. ) 
 B_SPLINE_CURVE_WITH_KNOTS ( ( 3, 2, 2, 2, 3 ),
 ( 0.1637931034482758563, 0.1666666666666666574, 0.1724137931034482873, 0.1781609195402298895, 0.1810344827586206906 ),
 .UNSPECIFIED. ) 
 CURVE ( )  GEOMETRIC_REPRESENTATION_ITEM ( )  RATIONAL_B_SPLINE_CURVE ( ( 0.9330127018922194093, 0.9330127018922194093, 1.000000000000000000, 0.8660254037844387076, 1.000000000000000000, 0.8660254037844387076, 1.000000000000000000, 0.9330127018922194093, 0.9330127018922194093 ) ) 
 REPRESENTATION_ITEM ( '' )  );
#13806 = CARTESIAN_POINT ( 'NONE',  ( -4.243569643749997233, -21.14050350850180138, -10.18177799141198747 ) ) ;
#13807 = MANIFOLD_SOLID_BREP ( 'LPattern6[3]', #10585 ) ;
#13808 = DIRECTION ( 'NONE',  ( -3.469446951953613696E-16, -0.000000000000000000, -1.000000000000000000 ) ) ;
#13809 = ORIENTED_EDGE ( 'NONE', *, *, #10323, .F. ) ;
#13810 = AXIS2_PLACEMENT_3D ( 'NONE', #2928, #11347, #13960 ) ;
#13811 = CARTESIAN_POINT ( 'NONE',  ( 4.000000000000003553, -22.51935735091492674, -11.90581315348016567 ) ) ;
#13812 = CARTESIAN_POINT ( 'NONE',  ( 4.000000000000003553, -23.22915819019439709, -12.91951380728103160 ) ) ;
#13813 = LINE ( 'NONE', #15126, #9564 ) ;
#13814 = ORIENTED_EDGE ( 'NONE', *, *, #2798, .T. ) ;
#13815 = CARTESIAN_POINT ( 'NONE',  ( -2.211161402132839182, 31.62819992234354416, 2.942372952327218627 ) ) ;
#13816 = CARTESIAN_POINT ( 'NONE',  ( -0.05938372350920064630, 23.87819992234354416, 3.680117784833935701 ) ) ;
#13817 = ADVANCED_FACE ( 'NONE', ( #4119, #9768 ), #14037, .T. ) ;
#13818 = CARTESIAN_POINT ( 'NONE',  ( 4.000000000000000888, -27.01371104396771017, -14.29809751472907919 ) ) ;
#13819 = CARTESIAN_POINT ( 'NONE',  ( 0.05938372350926800214, 29.87180007765648426, 2.628655560595669183 ) ) ;
#13820 = CARTESIAN_POINT ( 'NONE',  ( 0.05938372350919016857, 22.62819992234354416, -4.731580009072201776 ) ) ;
#13821 = UNCERTAINTY_MEASURE_WITH_UNIT (LENGTH_MEASURE( 1.000000000000000082E-05 ), #14889, 'distance_accuracy_value', 'NONE');
#13822 = CARTESIAN_POINT ( 'NONE',  ( 3.999999999999996447, -27.05567764914059481, -10.33171413117790394 ) ) ;
#13823 = EDGE_LOOP ( 'NONE', ( #132, #1592, #15054, #16688 ) ) ;
#13824 = CARTESIAN_POINT ( 'NONE',  ( 2.121784821874994176, -22.69489544611912279, -1.722954459712693787 ) ) ;
#13825 = AXIS2_PLACEMENT_3D ( 'NONE', #6418, #593, #13370 ) ;
#13826 = CARTESIAN_POINT ( 'NONE',  ( -2.864755990943265829, 25.74680007765647716, -2.011557305968488141 ) ) ;
#13827 =( LENGTH_UNIT ( ) NAMED_UNIT ( * ) SI_UNIT ( .MILLI., .METRE. ) );
#13828 = CARTESIAN_POINT ( 'NONE',  ( -2.121784821875005722, -27.86783793146007326, -9.110681959144070419 ) ) ;
#13829 = CARTESIAN_POINT ( 'NONE',  ( 8.000000000000000000, 0.000000000000000000, 0.000000000000000000 ) ) ;
#13830 = CARTESIAN_POINT ( 'NONE',  ( -1.734723475976807094E-15, 36.39999999999999147, -10.50000000000000178 ) ) ;
#13831 = DIRECTION ( 'NONE',  ( 1.000000000000000000, 0.000000000000000000, 0.000000000000000000 ) ) ;
#13832 = VERTEX_POINT ( 'NONE', #4295 ) ;
#13833 = ORIENTED_EDGE ( 'NONE', *, *, #4057, .T. ) ;
#13834 = CARTESIAN_POINT ( 'NONE',  ( -9.000000000000001776, 31.99999999999999289, 2.499999999999995559 ) ) ;
#13835 = PLANE ( 'NONE',  #3142 ) ;
#13836 = CARTESIAN_POINT ( 'NONE',  ( -1.071796769724496334, -21.27353689998724562, -13.07406643513510858 ) ) ;
#13837 = ORIENTED_EDGE ( 'NONE', *, *, #13411, .F. ) ;
#13838 = CARTESIAN_POINT ( 'NONE',  ( -0.05938372350921170689, 36.37819992234354771, 2.628655560595669183 ) ) ;
#13839 = CARTESIAN_POINT ( 'NONE',  ( -2.121784821874996396, -20.90060520497677743, -11.97491276323260756 ) ) ;
#13840 = CARTESIAN_POINT ( 'NONE',  ( 1.027846397803542144, 33.74680007765648071, -3.346150245485522312 ) ) ;
#13841 = CARTESIAN_POINT ( 'NONE',  ( -3.500000000000000444, 24.50319992234354416, -0.05647727720529563400 ) ) ;
#13842 = DIRECTION ( 'NONE',  ( 0.000000000000000000, 0.000000000000000000, -1.000000000000000000 ) ) ;
#13843 = CARTESIAN_POINT ( 'NONE',  ( 2.200000000000000178, 4.653657836759941744E-16, -3.799999999999999378 ) ) ;
#13844 = CARTESIAN_POINT ( 'NONE',  ( 4.243569643750000786, -24.28743054458419692, -10.40456545371456620 ) ) ;
#13845 = CLOSED_SHELL ( 'NONE', ( #5724, #4390, #10064, #15065, #12553, #9652, #8267, #13503, #1874, #8459 ) ) ;
#13846 = EDGE_CURVE ( 'NONE', #5635, #6645, #2907, .T. ) ;
#13847 = CIRCLE ( 'NONE', #15043, 0.9999999999999991118 ) ;
#13848 = ADVANCED_FACE ( 'NONE', ( #1526 ), #16087, .T. ) ;
#13849 = CIRCLE ( 'NONE', #14451, 0.9999999999999991118 ) ;
#13850 = CIRCLE ( 'NONE', #4365, 2.149999999999995470 ) ;
#13851 = CARTESIAN_POINT ( 'NONE',  ( -0.9009826423167719422, -10.00000000000000178, -12.54001985818077181 ) ) ;
#13852 = EDGE_CURVE ( 'NONE', #3584, #269, #15502, .T. ) ;
#13853 = CARTESIAN_POINT ( 'NONE',  ( -9.000000000000001776, 18.79999999999999361, 2.499999999999998224 ) ) ;
#13854 = DIRECTION ( 'NONE',  ( -1.028113302204112171E-14, 0.1129545544106649313, -0.9936001553129349961 ) ) ;
#13855 = CARTESIAN_POINT ( 'NONE',  ( 2.121784821875004390, -18.87874826683935936, -9.087401807113897334 ) ) ;
#13856 = CARTESIAN_POINT ( 'NONE',  ( -3.999999999999997335, -24.94988749924751303, -15.37696994014802065 ) ) ;
#13857 = CARTESIAN_POINT ( 'NONE',  ( -8.000000000000001776, 43.00000000000000000, 2.499999999999995115 ) ) ;
#13858 = EDGE_CURVE ( 'NONE', #12967, #9005, #11188, .T. ) ;
#13859 = CARTESIAN_POINT ( 'NONE',  ( 0.05938372350926800214, 39.87180007765647360, 2.628655560595669183 ) ) ;
#13860 = CARTESIAN_POINT ( 'NONE',  ( 3.999999999999996447, -25.31343922442924921, -7.843539797656847057 ) ) ;
#13861 = CARTESIAN_POINT ( 'NONE',  ( 3.500000000000000444, 34.24680007765648071, -0.05647727720536935281 ) ) ;
#13862 = CARTESIAN_POINT ( 'NONE',  ( -2.000000000000005773, -28.06608030478504290, -9.761559716304219592 ) ) ;
#13863 = TOROIDAL_SURFACE ( 'NONE', #16247, 9.000000000000001776, 0.9999999999999991118 ) ;
#13864 = CARTESIAN_POINT ( 'NONE',  ( -1.296796814808491183, 15.00000000000144240, -3.409573799784564763 ) ) ;
#13865 = TOROIDAL_SURFACE ( 'NONE', #8234, 9.000000000000003553, 0.9999999999999991118 ) ;
#13866 = ADVANCED_FACE ( 'NONE', ( #5955 ), #10213, .T. ) ;
#13867 = ORIENTED_EDGE ( 'NONE', *, *, #7437, .F. ) ;
#13868 = CARTESIAN_POINT ( 'NONE',  ( 4.243569643750000786, -20.93200839193060148, -5.612525994623947412 ) ) ;
#13869 = CARTESIAN_POINT ( 'NONE',  ( 1.027846397803542144, 21.24680007765647716, -3.346150245485522312 ) ) ;
#13870 = PRODUCT_DEFINITION ( 'UNKNOWN', '', #5972, #5624 ) ;
#13871 = CARTESIAN_POINT ( 'NONE',  ( 0.000000000000000000, 5.977523610840987267, 32.81826849749789687 ) ) ;
#13872 = CARTESIAN_POINT ( 'NONE',  ( 2.121784821874994176, -29.37347607688156259, -11.26095607540267807 ) ) ;
#13873 = CARTESIAN_POINT ( 'NONE',  ( 4.898587196589412829E-16, -10.00099999999999767, -4.000000000000000000 ) ) ;
#13874 = DIRECTION ( 'NONE',  ( -1.000000000000000000, 0.000000000000000000, 4.336808689942021680E-16 ) ) ;
#13876 = CARTESIAN_POINT ( 'NONE',  ( -1.734723475976807094E-15, 43.00000000000000000, -2.500000000000000000 ) ) ;
#13875 = AXIS2_PLACEMENT_3D ( 'NONE', #15032, #14763, #16515 ) ;
#13877 = CARTESIAN_POINT ( 'NONE',  ( -4.243569643749997233, -24.20555259025267603, -14.55912172808130656 ) ) ;
#13878 = ORIENTED_EDGE ( 'NONE', *, *, #15856, .F. ) ;
#13879 = CARTESIAN_POINT ( 'NONE',  ( -4.000000000000004441, -25.59305773644542370, -8.242876418240973280 ) ) ;
#13880 = CARTESIAN_POINT ( 'NONE',  ( 4.000000000000000888, -21.85152311680833748, -6.925729116128124474 ) ) ;
#13881 = CARTESIAN_POINT ( 'NONE',  ( -2.115076519116362519, 37.62180007765648071, 3.012182706137107147 ) ) ;
#13882 = VERTEX_POINT ( 'NONE', #13099 ) ;
#13883 = CARTESIAN_POINT ( 'NONE',  ( 3.999999999999996447, -24.28100163899738106, -6.369066117936657889 ) ) ;
#13884 =( REPRESENTATION_RELATIONSHIP ('NONE','NONE', #15868, #17791 ) REPRESENTATION_RELATIONSHIP_WITH_TRANSFORMATION ( #14915 )SHAPE_REPRESENTATION_RELATIONSHIP( ) );
#13885 =( NAMED_UNIT ( * ) PLANE_ANGLE_UNIT ( ) SI_UNIT ( $, .RADIAN. ) );
#13886 = CARTESIAN_POINT ( 'NONE',  ( -3.673772985318163098, 31.75319992234354771, 2.599342558261029001 ) ) ;
#13887 = DIRECTION ( 'NONE',  ( 0.000000000000000000, 0.000000000000000000, 1.000000000000000000 ) ) ;
#13888 = CARTESIAN_POINT ( 'NONE',  ( -2.518350579753611207, 29.37819992234355126, 0.7558219633769609480 ) ) ;
#13889 = EDGE_LOOP ( 'NONE', ( #12822, #16862, #12229, #872 ) ) ;
#13890 = CARTESIAN_POINT ( 'NONE',  ( 4.730628863548789710E-15, -22.01578123233109707, -15.70329423968597915 ) ) ;
#13891 = CARTESIAN_POINT ( 'NONE',  ( -3.607379964056306676, 27.74680007765648071, 2.690724712371306282 ) ) ;
#13892 = CARTESIAN_POINT ( 'NONE',  ( -1.999999999999996225, -17.57278640010649795, -6.854536663413863806 ) ) ;
#13893 = ORIENTED_EDGE ( 'NONE', *, *, #15458, .F. ) ;
#13894 = CARTESIAN_POINT ( 'NONE',  ( 0.000000000000000000, 0.000000000000000000, 0.000000000000000000 ) ) ;
#13895 = DIRECTION ( 'NONE',  ( -0.000000000000000000, -1.000000000000000000, -0.000000000000000000 ) ) ;
#13896 = DIRECTION ( 'NONE',  ( -1.000000000000000000, -0.000000000000000000, -0.000000000000000000 ) ) ;
#13897 = DIRECTION ( 'NONE',  ( 1.000000000000000000, 0.000000000000000000, 0.000000000000000000 ) ) ;
#13898 = VECTOR ( 'NONE', #4383, 1000.000000000000000 ) ;
#13899 = CARTESIAN_POINT ( 'NONE',  ( 4.243569643749996345, -25.28344594435018067, -7.555532749933418835 ) ) ;
#13900 = ORIENTED_EDGE ( 'NONE', *, *, #9442, .T. ) ;
#13901 = MANIFOLD_SOLID_BREP ( 'Cavity1', #5841 ) ;
#13902 = PRODUCT_DEFINITION_SHAPE ( 'NONE', 'NONE',  #18376 ) ;
#13903 = AXIS2_PLACEMENT_3D ( 'NONE', #15395, #9625, #6930 ) ;
#13904 = DIRECTION ( 'NONE',  ( -0.000000000000000000, 1.000000000000000000, -0.000000000000000000 ) ) ;
#13905 = EDGE_LOOP ( 'NONE', ( #3733, #8172, #6569, #4455 ) ) ;
#13906 = CARTESIAN_POINT ( 'NONE',  ( 4.000000000000003553, -22.26124795455695704, -11.53719473355011793 ) ) ;
#13907 = DIRECTION ( 'NONE',  ( -1.000000000000000000, -0.000000000000000000, -0.000000000000000000 ) ) ;
#13908 = CARTESIAN_POINT ( 'NONE',  ( -1.135272562821090014, 15.99680007765647716, -3.311245368580554072 ) ) ;
#13909 = ORIENTED_EDGE ( 'NONE', *, *, #9977, .F. ) ;
#13910 = CARTESIAN_POINT ( 'NONE',  ( -3.518350579753605434, 31.87819992234354416, 1.080741659609877781 ) ) ;
#13911 = CARTESIAN_POINT ( 'NONE',  ( -2.798362969681409851, 17.25319992234354416, -2.102939460078765421 ) ) ;
#13912 = CARTESIAN_POINT ( 'NONE',  ( -5.330712181944245322E-15, -23.94572221871285578, -1.373575165951426369 ) ) ;
#13913 = CARTESIAN_POINT ( 'NONE',  ( -1.989345975306426206, 27.74680007765648071, 1.515154207786343799 ) ) ;
#13914 = CARTESIAN_POINT ( 'NONE',  ( -3.673772985318163098, 29.25319992234354416, 2.599342558261029001 ) ) ;
#13915 = CARTESIAN_POINT ( 'NONE',  ( 4.000000000000003553, -22.97104879383642384, -12.55089538735098387 ) ) ;
#13916 = VERTEX_POINT ( 'NONE', #9114 ) ;
#13917 = TOROIDAL_SURFACE ( 'NONE', #10657, 4.400000000000002132, 0.4000000000000000222 ) ;
#13918 = CARTESIAN_POINT ( 'NONE',  ( 4.243569643750000786, -19.89957080649872623, -4.138052314903757356 ) ) ;
#13919 = AXIS2_PLACEMENT_3D ( 'NONE', #13894, #1205, #13983 ) ;
#13920 = CARTESIAN_POINT ( 'NONE',  ( 1.135272562821090458, 19.74680007765648071, 3.311245368580554072 ) ) ;
#13921 =( BOUNDED_CURVE ( )  B_SPLINE_CURVE ( 2, ( #2713, #5565, #10854, #16532, #1228, #8071, #2620, #16632, #7983 ),
 .UNSPECIFIED., .F., .F. ) 
 B_SPLINE_CURVE_WITH_KNOTS ( ( 3, 2, 2, 2, 3 ),
 ( 0.1810344827586206906, 0.1839080459770114917, 0.1896551724137930939, 0.1954022988505747238, 0.1982758620689655249 ),
 .UNSPECIFIED. ) 
 CURVE ( )  GEOMETRIC_REPRESENTATION_ITEM ( )  RATIONAL_B_SPLINE_CURVE ( ( 0.9330127018922194093, 0.9330127018922194093, 1.000000000000000000, 0.8660254037844387076, 1.000000000000000000, 0.8660254037844387076, 1.000000000000000000, 0.9330127018922194093, 0.9330127018922194093 ) ) 
 REPRESENTATION_ITEM ( '' )  );
#13922 = CARTESIAN_POINT ( 'NONE',  ( -1.661723472263481630E-14, -21.09148155414254688, -12.81406445585025544 ) ) ;
#13923 = CARTESIAN_POINT ( 'NONE',  ( 4.243569643750000786, -22.96461988824960443, -8.515396051573073777 ) ) ;
#13924 = EDGE_CURVE ( 'NONE', #15144, #13588, #11775, .T. ) ;
#13925 = LINE ( 'NONE', #959, #610 ) ;
#13926 =( NAMED_UNIT ( * ) PLANE_ANGLE_UNIT ( ) SI_UNIT ( $, .RADIAN. ) );
#13927 = CARTESIAN_POINT ( 'NONE',  ( 9.000000000000001776, 20.99999999999999289, -2.500000000000002665 ) ) ;
#13928 = ORIENTED_EDGE ( 'NONE', *, *, #319, .T. ) ;
#13929 = ORIENTED_EDGE ( 'NONE', *, *, #11343, .F. ) ;
#13930 = CARTESIAN_POINT ( 'NONE',  ( -2.864755990943265829, 15.74680007765647716, -2.011557305968488141 ) ) ;
#13931 = CYLINDRICAL_SURFACE ( 'NONE', #6683, 4.000000000000000000 ) ;
#13932 = DIRECTION ( 'NONE',  ( 0.000000000000000000, 0.000000000000000000, -1.000000000000000000 ) ) ;
#13933 = ORIENTED_EDGE ( 'NONE', *, *, #9265, .T. ) ;
#13934 = CIRCLE ( 'NONE', #3855, 0.9999999999999991118 ) ;
#13935 = CARTESIAN_POINT ( 'NONE',  ( 0.05938372350921204690, 32.62819992234354771, -2.628655560595669183 ) ) ;
#13936 = CARTESIAN_POINT ( 'NONE',  ( 4.243569643749996345, -26.79983864795324422, -9.721165967022450616 ) ) ;
#13937 = CARTESIAN_POINT ( 'NONE',  ( -1.027846397803541700, 27.49680007765648071, 3.346150245485522312 ) ) ;
#13938 = CARTESIAN_POINT ( 'NONE',  ( -1.027846397803611866, 30.00319992234354416, -3.346150245485499219 ) ) ;
#13939 = CARTESIAN_POINT ( 'NONE',  ( 0.000000000000000000, 9.254131787996968228, 30.52396275209373044 ) ) ;
#13940 = DIRECTION ( 'NONE',  ( -1.000000000000000000, 0.000000000000000000, 4.336808689942021680E-16 ) ) ;
#13941 = CARTESIAN_POINT ( 'NONE',  ( 4.243569643749996345, -25.54155534070815392, -7.924151169863466571 ) ) ;
#13942 = CARTESIAN_POINT ( 'NONE',  ( 0.8866433558360066192, -9.999999999998044231, -3.510284692354058045 ) ) ;
#13943 = CARTESIAN_POINT ( 'NONE',  ( -13.00000000000000178, 13.00000000000000178, 25.00000000000000355 ) ) ;
#13944 = CARTESIAN_POINT ( 'NONE',  ( -3.706921591972381904E-14, -18.96207903348436119, -9.772962490420598058 ) ) ;
#13945 = CARTESIAN_POINT ( 'NONE',  ( -4.243569643750000786, -21.54501820828076930, -6.487994741957813005 ) ) ;
#13946 = LINE ( 'NONE', #5506, #6789 ) ;
#13947 = SURFACE_SIDE_STYLE ('',( #15705 ) ) ;
#13948 = CARTESIAN_POINT ( 'NONE',  ( 0.05938372350921204690, 15.12819992234354771, -2.628655560595669183 ) ) ;
#13949 = CYLINDRICAL_SURFACE ( 'NONE', #18046, 0.9999999999999991118 ) ;
#13950 = CARTESIAN_POINT ( 'NONE',  ( 0.05938372350927906967, 39.87180007765648071, 3.680117784833935701 ) ) ;
#13951 = DIRECTION ( 'NONE',  ( -0.000000000000000000, -0.5735764363510414965, -0.8191520442889950182 ) ) ;
#13952 = ADVANCED_FACE ( 'NONE', ( #17589 ), #13863, .T. ) ;
#13953 = DIRECTION ( 'NONE',  ( 0.8191520442889951292, 0.4698463103929519935, -0.3289899283371605643 ) ) ;
#13954 = ORIENTED_EDGE ( 'NONE', *, *, #8396, .F. ) ;
#13955 = B_SPLINE_CURVE_WITH_KNOTS ( 'NONE', 3,
 ( #780, #6612, #2271, #5310, #10962, #16645, #13648, #3648, #14885, #967, #17942, #4939, #5214, #17677 ),
 .UNSPECIFIED., .F., .F.,
 ( 4, 2, 2, 2, 2, 2, 4 ),
 ( 0.000000000000000000, 0.002175243210657258879, 0.004350486421314517758, 0.008700972842629035517, 0.01087621605328629310, 0.01305145926394355588, 0.01740194568525808144 ),
 .UNSPECIFIED. ) ;
#13956 = CARTESIAN_POINT ( 'NONE',  ( -5.330712181944246111E-15, -26.04286106412135027, -4.368599827883064890 ) ) ;
#13957 = CARTESIAN_POINT ( 'NONE',  ( 2.798362969681366330, 31.49680007765647716, -2.102939460078824929 ) ) ;
#13958 = DIRECTION ( 'NONE',  ( -3.469446951953613696E-16, -0.000000000000000000, -1.000000000000000000 ) ) ;
#13959 = PLANE ( 'NONE',  #10021 ) ;
#13960 = DIRECTION ( 'NONE',  ( 0.000000000000000000, -0.000000000000000000, 1.000000000000000000 ) ) ;
#13961 = CARTESIAN_POINT ( 'NONE',  ( -9.000000000000001776, 20.99999999999999289, 2.499999999999998224 ) ) ;
#13962 = DIRECTION ( 'NONE',  ( 0.000000000000000000, 0.000000000000000000, 1.000000000000000000 ) ) ;
#13963 = CARTESIAN_POINT ( 'NONE',  ( 2.121784821875004390, -23.26660800492483006, -15.35391494592470885 ) ) ;
#13964 = VERTEX_POINT ( 'NONE', #13287 ) ;
#13965 = DIRECTION ( 'NONE',  ( 0.000000000000000000, 1.000000000000000000, 0.000000000000000000 ) ) ;
#13966 = CARTESIAN_POINT ( 'NONE',  ( -4.000000000000004441, -23.85081931173408165, -5.754702084719914623 ) ) ;
#13967 = CARTESIAN_POINT ( 'NONE',  ( -3.481649420246369697, 37.87180007765648071, 1.193696214020542490 ) ) ;
#13968 = VERTEX_POINT ( 'NONE', #1709 ) ;
#13969 = CARTESIAN_POINT ( 'NONE',  ( 1.071796769724490339, -22.13544584029325435, -14.30499997022636727 ) ) ;
#13970 = ADVANCED_FACE ( 'NONE', ( #7343, #13003, #11890, #15893, #3190, #8829 ), #7535, .F. ) ;
#13971 = EDGE_CURVE ( 'NONE', #16888, #17673, #3380, .T. ) ;
#13972 = CIRCLE ( 'NONE', #965, 0.1999999999999987899 ) ;
#13973 =( NAMED_UNIT ( * ) PLANE_ANGLE_UNIT ( ) SI_UNIT ( $, .RADIAN. ) );
#13974 = CARTESIAN_POINT ( 'NONE',  ( -4.499999999999999112, 15.49680007765647538, 0.05647727720537927543 ) ) ;
#13975 = CARTESIAN_POINT ( 'NONE',  ( 4.000000000000000000, 3.518949890710770134, -4.119968255444916849E-15 ) ) ;
#13976 = EDGE_CURVE ( 'NONE', #10092, #5374, #6459, .T. ) ;
#13977 = CARTESIAN_POINT ( 'NONE',  ( -1.497042530366522461, 34.87819992234354771, -2.161531897785030409 ) ) ;
#13978 = ORIENTED_EDGE ( 'NONE', *, *, #6010, .F. ) ;
#13979 = CARTESIAN_POINT ( 'NONE',  ( -2.121784821875005722, -28.15821100236278696, -9.525377681565375454 ) ) ;
#13980 = CARTESIAN_POINT ( 'NONE',  ( 4.518350579753633411, 21.87180007765647360, 1.405661355842698468 ) ) ;
#13981 = EDGE_LOOP ( 'NONE', ( #17390, #14289 ) ) ;
#13982 = B_SPLINE_CURVE_WITH_KNOTS ( 'NONE', 3,
 ( #18064, #13671, #16666, #6635, #15271, #15362, #12281, #16848, #5336, #17970, #5239, #2480, #10896, #3945, #9595, #2570, #11074, #13864, #1171, #18155, #2660, #1265, #8294, #6900 ),
 .UNSPECIFIED., .F., .F.,
 ( 4, 2, 2, 2, 2, 2, 2, 2, 2, 2, 2, 4 ),
 ( 0.000000000000000000, 0.0006232196737604741134, 0.001246439347520948227, 0.001869659021281422882, 0.002492878695041897321, 0.003116098368802372193, 0.003739318042562846632, 0.004362537716323321504, 0.004674147553203558507, 0.004829952471643678309, 0.004907854930863738210, 0.004985757390083797244 ),
 .UNSPECIFIED. ) ;
#13983 = DIRECTION ( 'NONE',  ( 0.000000000000000000, 0.000000000000000000, 1.000000000000000000 ) ) ;
#13984 = PRESENTATION_STYLE_ASSIGNMENT (( #16699 ) ) ;
#13985 = DIRECTION ( 'NONE',  ( -0.000000000000000000, 1.000000000000000000, -0.000000000000000000 ) ) ;
#13986 = LINE ( 'NONE', #8326, #589 ) ;
#13987 = PRESENTATION_LAYER_ASSIGNMENT (  '', '', ( #16081 ) ) ;
#13988 = CARTESIAN_POINT ( 'NONE',  ( -4.243569643749997233, -20.36617531942789228, -9.075922731621842487 ) ) ;
#13989 = ORIENTED_EDGE ( 'NONE', *, *, #5917, .T. ) ;
#13990 = CARTESIAN_POINT ( 'NONE',  ( -2.451037035742412051, -29.65081295030892505, -12.49886881493011437 ) ) ;
#13991 = ORIENTED_EDGE ( 'NONE', *, *, #14255, .F. ) ;
#13992 = CARTESIAN_POINT ( 'NONE',  ( 4.000000000000003553, -22.77746674727289289, -12.27443157341021163 ) ) ;
#13993 = CARTESIAN_POINT ( 'NONE',  ( 2.000000000000004441, -22.26177376727626367, -13.55110462547639472 ) ) ;
#13994 = CARTESIAN_POINT ( 'NONE',  ( -8.500000000000010658, 15.00000000000000000, 20.49999999999998934 ) ) ;
#13995 = CARTESIAN_POINT ( 'NONE',  ( 4.499999999999999112, 15.75319992234354416, 0.05647727720528474687 ) ) ;
#13996 = CARTESIAN_POINT ( 'NONE',  ( -2.798362969681409851, 22.25319992234354416, -2.102939460078765421 ) ) ;
#13997 = CARTESIAN_POINT ( 'NONE',  ( 3.999999999999996447, -28.66886137708284110, -12.63557925674746762 ) ) ;
#13998 = CARTESIAN_POINT ( 'NONE',  ( -2.518350579753628526, 28.12180007765647716, -0.7558219633769075463 ) ) ;
#13999 = CIRCLE ( 'NONE', #391, 3.047499999999999876 ) ;
#14000 = CARTESIAN_POINT ( 'NONE',  ( 3.673772985318163098, 25.50319992234354416, -2.599342558261029001 ) ) ;
#14001 =( GEOMETRIC_REPRESENTATION_CONTEXT ( 3 ) GLOBAL_UNCERTAINTY_ASSIGNED_CONTEXT ( ( #15289 ) ) GLOBAL_UNIT_ASSIGNED_CONTEXT ( ( #12980, #295, #10191 ) ) REPRESENTATION_CONTEXT ( 'NONE', 'WORKASPACE' ) );
#14002 = UNCERTAINTY_MEASURE_WITH_UNIT (LENGTH_MEASURE( 1.000000000000000082E-05 ), #2985, 'distance_accuracy_value', 'NONE');
#14003 = CARTESIAN_POINT ( 'NONE',  ( -4.000000000000000888, -23.20659744698271965, -8.860975819754113303 ) ) ;
#14004 = ORIENTED_EDGE ( 'NONE', *, *, #4226, .T. ) ;
#14005 = EDGE_CURVE ( 'NONE', #12491, #4433, #13563, .T. ) ;
#14006 = CARTESIAN_POINT ( 'NONE',  ( 2.864755990943265829, 21.99680007765647716, 2.011557305968487697 ) ) ;
#14007 = CARTESIAN_POINT ( 'NONE',  ( -1.071796769724486564, -27.52716991099435973, -8.057605589732816043 ) ) ;
#14008 = CARTESIAN_POINT ( 'NONE',  ( 2.121784821874994176, -26.53427271694390299, -7.206153456172153859 ) ) ;
#14009 = VECTOR ( 'NONE', #14249, 1000.000000000000000 ) ;
#14010 = CARTESIAN_POINT ( 'NONE',  ( 2.000000000000004441, -21.48744557820235457, -12.44524936568625151 ) ) ;
#14011 = AXIS2_PLACEMENT_3D ( 'NONE', #2520, #12593, #18107 ) ;
#14013 = FACE_OUTER_BOUND ( 'NONE', #7956, .T. ) ;
#14012 = MECHANICAL_DESIGN_GEOMETRIC_PRESENTATION_REPRESENTATION (  '', ( #6355 ), #3087 ) ;
#14014 = CARTESIAN_POINT ( 'NONE',  ( -4.000000000000000888, -23.27112479677715839, -8.953130425743392351 ) ) ;
#14015 = ORIENTED_EDGE ( 'NONE', *, *, #1047, .T. ) ;
#14016 = ORIENTED_EDGE ( 'NONE', *, *, #14431, .T. ) ;
#14017 = CARTESIAN_POINT ( 'NONE',  ( 1.027846397803542144, 26.24680007765648071, -3.346150245485522312 ) ) ;
#14018 = CARTESIAN_POINT ( 'NONE',  ( -3.999999999999997335, -20.04580896844610649, -8.373219961477113671 ) ) ;
#14019 = FACE_OUTER_BOUND ( 'NONE', #3871, .T. ) ;
#14020 = DIRECTION ( 'NONE',  ( 0.000000000000000000, 0.000000000000000000, -1.000000000000000000 ) ) ;
#14021 = ORIENTED_EDGE ( 'NONE', *, *, #15325, .T. ) ;
#14022 = CARTESIAN_POINT ( 'NONE',  ( -0.7188294034286550893, 37.50319992234354771, -2.395093729190349130 ) ) ;
#14023 = CARTESIAN_POINT ( 'NONE',  ( 2.121784821875004390, -20.42740464498717401, -11.29911232669418197 ) ) ;
#14024 = CARTESIAN_POINT ( 'NONE',  ( 3.481649420246369697, 31.62180007765647360, -1.193696214020541824 ) ) ;
#14025 = EDGE_CURVE ( 'NONE', #18076, #17255, #18118, .T. ) ;
#14026 = CARTESIAN_POINT ( 'NONE',  ( 2.115076519116426024, 26.12819992234354771, 3.012182706137062294 ) ) ;
#14027 = CARTESIAN_POINT ( 'NONE',  ( -3.706921591972381904E-14, -17.99416879784692469, -8.390643416689682610 ) ) ;
#14028 = EDGE_CURVE ( 'NONE', #6628, #7899, #9474, .T. ) ;
#14029 = CYLINDRICAL_SURFACE ( 'NONE', #1375, 7.499999999999999112 ) ;
#14030 = AXIS2_PLACEMENT_3D ( 'NONE', #2371, #15340, #13754 ) ;
#14031 = CARTESIAN_POINT ( 'NONE',  ( 4.730628863548789710E-15, -20.20901545782531628, -13.12296530017564500 ) ) ;
#14032 = LINE ( 'NONE', #12358, #204 ) ;
#14033 = DIRECTION ( 'NONE',  ( -3.469446951953613696E-16, -0.000000000000000000, -1.000000000000000000 ) ) ;
#14034 = DIRECTION ( 'NONE',  ( 0.000000000000000000, 0.000000000000000000, 1.000000000000000000 ) ) ;
#14035 = CARTESIAN_POINT ( 'NONE',  ( -5.330712181944245322E-15, -25.49437859686066332, -3.585285685531713451 ) ) ;
#14036 = CARTESIAN_POINT ( 'NONE',  ( -1.999999999999996225, -24.02552130905571204, -16.06999716166505721 ) ) ;
#14037 = PLANE ( 'NONE',  #8819 ) ;
#14038 = CARTESIAN_POINT ( 'NONE',  ( 0.8262555684460829442, 15.25319992234354771, -2.360188852285421302 ) ) ;
#14039 = DIRECTION ( 'NONE',  ( -0.000000000000000000, -0.5735764363510414965, -0.8191520442889950182 ) ) ;
#14040 = LINE ( 'NONE', #11251, #61 ) ;
#14041 = DIRECTION ( 'NONE',  ( 0.000000000000000000, 0.8660254037844380415, -0.5000000000000012212 ) ) ;
#14042 = CARTESIAN_POINT ( 'NONE',  ( -9.831267214419536771, -9.942687138680838643, 1.765148412673711142 ) ) ;
#14043 = EDGE_CURVE ( 'NONE', #7315, #14839, #17524, .T. ) ;
#14044 = ORIENTED_EDGE ( 'NONE', *, *, #314, .F. ) ;
#14045 = CARTESIAN_POINT ( 'NONE',  ( 2.121784821875004390, -18.39479314866817461, -8.396242269745057385 ) ) ;
#14046 = CARTESIAN_POINT ( 'NONE',  ( -3.500000000000000444, 30.49680007765647716, 0.05647727720536892260 ) ) ;
#14047 = FILL_AREA_STYLE ('',( #7174 ) ) ;
#14048 = DIRECTION ( 'NONE',  ( 0.000000000000000000, -0.000000000000000000, -1.000000000000000000 ) ) ;
#14049 = DIRECTION ( 'NONE',  ( 0.000000000000000000, 0.000000000000000000, 1.000000000000000000 ) ) ;
#14050 = CARTESIAN_POINT ( 'NONE',  ( 3.999999999999996447, -28.34622463093043621, -12.17480623082814262 ) ) ;
#14051 = CARTESIAN_POINT ( 'NONE',  ( 15.00000000000000355, -10.00000000000000000, 30.00000000000000000 ) ) ;
#14052 = CARTESIAN_POINT ( 'NONE',  ( -4.243569643749997233, -24.72177138296861898, -15.29635856794139848 ) ) ;
#14053 = ORIENTED_EDGE ( 'NONE', *, *, #8797, .F. ) ;
#14054 = CARTESIAN_POINT ( 'NONE',  ( -1.071796769724486564, -26.94642376848398158, -7.228214143883440634 ) ) ;
#14055 = CARTESIAN_POINT ( 'NONE',  ( 4.000000000000003553, -20.19637278369320299, -8.588247374109736043 ) ) ;
#14056 = CARTESIAN_POINT ( 'NONE',  ( -0.05938372350927861171, 36.12180007765648782, -3.680117784833935701 ) ) ;
#14057 = VERTEX_POINT ( 'NONE', #9382 ) ;
#14058 = FACE_OUTER_BOUND ( 'NONE', #9567, .T. ) ;
#14059 = CARTESIAN_POINT ( 'NONE',  ( -0.05938372350918959958, 38.87819992234354771, 4.731580009072201776 ) ) ;
#14060 = DIRECTION ( 'NONE',  ( 0.000000000000000000, 0.000000000000000000, -1.000000000000000000 ) ) ;
#14061 = CARTESIAN_POINT ( 'NONE',  ( 2.481649420246391902, 35.87819992234354771, 0.8687765177875720335 ) ) ;
#14062 = ORIENTED_EDGE ( 'NONE', *, *, #14608, .F. ) ;
#14063 = CARTESIAN_POINT ( 'NONE',  ( -5.330712181944246111E-15, -29.14017382041697957, -8.792020867043637722 ) ) ;
#14064 = CARTESIAN_POINT ( 'NONE',  ( 2.829195390882805583, 37.12180007765647360, 3.793023760679204770 ) ) ;
#14065 = VERTEX_POINT ( 'NONE', #3732 ) ;
#14066 =( NAMED_UNIT ( * ) PLANE_ANGLE_UNIT ( ) SI_UNIT ( $, .RADIAN. ) );
#14067 = FACE_OUTER_BOUND ( 'NONE', #15684, .T. ) ;
#14068 =( BOUNDED_CURVE ( )  B_SPLINE_CURVE ( 3, ( #17482, #11504, #4649, #8818 ),
 .UNSPECIFIED., .F., .T. ) 
 B_SPLINE_CURVE_WITH_KNOTS ( ( 4, 4 ),
 ( 4.712388980384689674, 6.283185307179586232 ),
 .UNSPECIFIED. ) 
 CURVE ( )  GEOMETRIC_REPRESENTATION_ITEM ( )  RATIONAL_B_SPLINE_CURVE ( ( 1.000000000000000000, 0.8047378541243649375, 0.8047378541243649375, 1.000000000000000000 ) ) 
 REPRESENTATION_ITEM ( '' )  );
#14069 = EDGE_CURVE ( 'NONE', #5475, #4719, #9207, .T. ) ;
#14070 = CARTESIAN_POINT ( 'NONE',  ( -8.500000000000007105, 15.00000000000000000, -20.49999999999999645 ) ) ;
#14071 = DIRECTION ( 'NONE',  ( -0.000000000000000000, -1.000000000000000000, -0.000000000000000000 ) ) ;
#14072 = EDGE_CURVE ( 'NONE', #2835, #10774, #13955, .T. ) ;
#14073 = CARTESIAN_POINT ( 'NONE',  ( 4.243569643750000786, -22.99688356279435197, -8.561473354064329300 ) ) ;
#14074 = EDGE_LOOP ( 'NONE', ( #12404, #14378, #12320 ) ) ;
#14075 = EDGE_CURVE ( 'NONE', #9076, #5876, #7935, .T. ) ;
#14076 = DIRECTION ( 'NONE',  ( 0.000000000000000000, 0.000000000000000000, 1.000000000000000000 ) ) ;
#14077 = ORIENTED_EDGE ( 'NONE', *, *, #3605, .T. ) ;
#14078 = CARTESIAN_POINT ( 'NONE',  ( 2.000000000000004441, -22.32630111707070242, -13.64325923146567199 ) ) ;
#14079 = VECTOR ( 'NONE', #4746, 1000.000000000000000 ) ;
#14080 = CARTESIAN_POINT ( 'NONE',  ( 3.579096709490575479E-14, -23.64400226490599266, -2.511867456126184894 ) ) ;
#14081 = DIRECTION ( 'NONE',  ( -0.000000000000000000, -0.000000000000000000, -1.000000000000000000 ) ) ;
#14082 =( NAMED_UNIT ( * ) SI_UNIT ( $, .STERADIAN. ) SOLID_ANGLE_UNIT ( ) );
#14083 = ADVANCED_FACE ( 'NONE', ( #15150 ), #13554, .F. ) ;
#14084 = CARTESIAN_POINT ( 'NONE',  ( -2.829195390882724315, 21.62819992234354416, 3.793023760679264722 ) ) ;
#14085 = CARTESIAN_POINT ( 'NONE',  ( -1.027846397803611866, 17.50319992234354416, -3.346150245485499219 ) ) ;
#14086 = CARTESIAN_POINT ( 'NONE',  ( -5.279047395330986450E-15, -30.34552082656112759, -11.00377920042669722 ) ) ;
#14087 = AXIS2_PLACEMENT_3D ( 'NONE', #4975, #14828, #10631 ) ;
#14088 = CARTESIAN_POINT ( 'NONE',  ( 0.05938372350926800214, 34.87180007765648071, 2.628655560595669183 ) ) ;
#14089 = CARTESIAN_POINT ( 'NONE',  ( -0.05938372350918959958, 33.87819992234354061, 4.731580009072201776 ) ) ;
#14090 = CARTESIAN_POINT ( 'NONE',  ( 3.999999999999996447, -26.02324006370871601, -8.857240451457712993 ) ) ;
#14091 = ORIENTED_EDGE ( 'NONE', *, *, #10523, .F. ) ;
#14092 = EDGE_CURVE ( 'NONE', #15689, #13741, #694, .T. ) ;
#14093 = CARTESIAN_POINT ( 'NONE',  ( 2.000000000000004441, -17.93844137898523527, -7.376746092654861364 ) ) ;
#14094 = CARTESIAN_POINT ( 'NONE',  ( 3.518350579753631191, 19.37180007765648071, 1.080741659609802285 ) ) ;
#14095 = CIRCLE ( 'NONE', #14392, 0.9999999999999991118 ) ;
#14096 = FILL_AREA_STYLE ('',( #3998 ) ) ;
#14097 = PRODUCT_RELATED_PRODUCT_CATEGORY ( 'part', '', ( #1911 ) ) ;
#14098 = CARTESIAN_POINT ( 'NONE',  ( -4.243569643750000786, -22.83556519007061425, -8.331086841608051685 ) ) ;
#14099 = TOROIDAL_SURFACE ( 'NONE', #3739, 4.400000000000002132, 0.4000000000000000222 ) ;
#14100 = CARTESIAN_POINT ( 'NONE',  ( -1.336863392178478716, 24.99680007765647716, 4.297206761780677731 ) ) ;
#14101 = CARTESIAN_POINT ( 'NONE',  ( -11.99999999999999822, 13.00000000000000178, 15.00000000000000000 ) ) ;
#14102 = CARTESIAN_POINT ( 'NONE',  ( 1.300000000000000044, -1.443375672974064328, 1.278502688459867223E-18 ) ) ;
#14103 = LINE ( 'NONE', #15327, #11487 ) ;
#14104 = ORIENTED_EDGE ( 'NONE', *, *, #10144, .F. ) ;
#14105 = ORIENTED_EDGE ( 'NONE', *, *, #10176, .F. ) ;
#14106 = CARTESIAN_POINT ( 'NONE',  ( -3.518350579753630747, 23.12180007765647716, -1.080741659609802729 ) ) ;
#14107 = DIRECTION ( 'NONE',  ( 1.000000000000000000, 0.000000000000000000, -4.336808689942021680E-16 ) ) ;
#14108 = DIRECTION ( 'NONE',  ( -0.000000000000000000, -1.000000000000000000, -0.000000000000000000 ) ) ;
#14109 = CARTESIAN_POINT ( 'NONE',  ( 1.071796769724495224, -17.74758610220779431, -8.038486831415553979 ) ) ;
#14110 = CARTESIAN_POINT ( 'NONE',  ( -3.999999999999997335, -25.01441484904194823, -15.46912454613729793 ) ) ;
#14111 = ORIENTED_EDGE ( 'NONE', *, *, #17675, .T. ) ;
#14112 = CARTESIAN_POINT ( 'NONE',  ( 1.135272562821020070, 22.75319992234354416, -3.311245368580577164 ) ) ;
#14113 = CARTESIAN_POINT ( 'NONE',  ( 2.121784821874994176, -25.75994452787000100, -6.100298196382009763 ) ) ;
#14114 = CARTESIAN_POINT ( 'NONE',  ( -3.481649420246369697, 40.37180007765648071, 1.193696214020542490 ) ) ;
#14115 = CARTESIAN_POINT ( 'NONE',  ( -2.115076519116425580, 27.37819992234354771, -3.012182706137062738 ) ) ;
#14116 = CARTESIAN_POINT ( 'NONE',  ( 7.056670106005041632, -10.00000000000000178, -9.351700598554229416 ) ) ;
#14117 = AXIS2_PLACEMENT_3D ( 'NONE', #882, #14804, #7731 ) ;
#14118 = CARTESIAN_POINT ( 'NONE',  ( -1.734723475976807094E-15, 16.59999999999999787, -2.500000000000000000 ) ) ;
#14119 = CARTESIAN_POINT ( 'NONE',  ( 2.121784821875004390, -21.49210590496380036, -12.81966330890563022 ) ) ;
#14120 = DIRECTION ( 'NONE',  ( 0.000000000000000000, 0.000000000000000000, -1.000000000000000000 ) ) ;
#14121 = DIRECTION ( 'NONE',  ( -0.000000000000000000, -1.000000000000000000, -0.000000000000000000 ) ) ;
#14122 = CARTESIAN_POINT ( 'NONE',  ( 8.500000000000019540, 0.000000000000000000, -20.49999999999998934 ) ) ;
#14123 = VECTOR ( 'NONE', #8371, 1000.000000000000000 ) ;
#14124 = CARTESIAN_POINT ( 'NONE',  ( 4.243569643750003451, -19.12940112854596819, -7.309626136123695161 ) ) ;
#14125 = CYLINDRICAL_SURFACE ( 'NONE', #8276, 2.149999999999995470 ) ;
#14126 = CARTESIAN_POINT ( 'NONE',  ( -8.500000000000005329, 10.00000000000000000, -20.49999999999999645 ) ) ;
#14127 = ORIENTED_EDGE ( 'NONE', *, *, #15232, .T. ) ;
#14128 = CARTESIAN_POINT ( 'NONE',  ( 2.055738996568281518, 18.00319992234354416, -1.423772053676066518 ) ) ;
#14129 = CARTESIAN_POINT ( 'NONE',  ( -2.121784821874996396, -23.48169916855646733, -15.66109696253308314 ) ) ;
#14130 = CARTESIAN_POINT ( 'NONE',  ( -2.115076519116362519, 35.12180007765646650, 3.012182706137108035 ) ) ;
#14131 = FACE_BOUND ( 'NONE', #3645, .T. ) ;
#14132 = DIRECTION ( 'NONE',  ( -0.000000000000000000, -1.000000000000000000, -0.000000000000000000 ) ) ;
#14133 = EDGE_LOOP ( 'NONE', ( #17444, #653, #8405, #12425 ) ) ;
#14134 = CARTESIAN_POINT ( 'NONE',  ( -15.00000000000000178, 10.00000000000000000, 24.99999999999999645 ) ) ;
#14135 = CARTESIAN_POINT ( 'NONE',  ( 1.027846397803542144, 28.74680007765647716, -3.346150245485522312 ) ) ;
#14136 = CIRCLE ( 'NONE', #18311, 2.149999999999995470 ) ;
#14137 = VECTOR ( 'NONE', #9154, 999.9999999999998863 ) ;
#14138 = PRESENTATION_STYLE_ASSIGNMENT (( #14328 ) ) ;
#14139 = CARTESIAN_POINT ( 'NONE',  ( -5.330712181944246111E-15, -30.14034773130410372, -10.22041724427257137 ) ) ;
#14140 = DIRECTION ( 'NONE',  ( -4.915049848600951133E-16, 0.000000000000000000, -1.000000000000000000 ) ) ;
#14141 = CARTESIAN_POINT ( 'NONE',  ( 4.000000000000000000, -2.639212418033074492, 1.523750000000003046 ) ) ;
#14142 = EDGE_CURVE ( 'NONE', #16574, #14161, #8231, .T. ) ;
#14143 = CARTESIAN_POINT ( 'NONE',  ( 0.000000000000000000, 0.7216878364870329410, -1.250000000000000000 ) ) ;
#14144 = CARTESIAN_POINT ( 'NONE',  ( -4.243569643750005227, -26.62776571704792161, -9.475420353735755086 ) ) ;
#14145 = ORIENTED_EDGE ( 'NONE', *, *, #15907, .T. ) ;
#14146 = DIRECTION ( 'NONE',  ( 0.000000000000000000, 1.000000000000000000, 0.000000000000000000 ) ) ;
#14147 = CARTESIAN_POINT ( 'NONE',  ( 4.000000000000000888, -20.30286673866052283, -4.714018596547838946 ) ) ;
#14148 = AXIS2_PLACEMENT_3D ( 'NONE', #599, #3469, #8729 ) ;
#14149 = CARTESIAN_POINT ( 'NONE',  ( -2.500000000000001332, 17.99680007765648071, 0.05647727720535858364 ) ) ;
#14150 = PRODUCT_DEFINITION_CONTEXT ( 'detailed design', #6307, 'design' ) ;
#14151 = AXIS2_PLACEMENT_3D ( 'NONE', #11168, #16860, #4136 ) ;
#14152 = ORIENTED_EDGE ( 'NONE', *, *, #964, .F. ) ;
#14153 = DIRECTION ( 'NONE',  ( -1.000000000000000000, 0.000000000000000000, 4.336808689942021680E-16 ) ) ;
#14154 =( LENGTH_UNIT ( ) NAMED_UNIT ( * ) SI_UNIT ( .MILLI., .METRE. ) );
#14155 = DIRECTION ( 'NONE',  ( -0.000000000000000000, -1.000000000000000000, -0.000000000000000000 ) ) ;
#14156 = CARTESIAN_POINT ( 'NONE',  ( 2.481649420246391902, 33.37819992234354771, 0.8687765177875720335 ) ) ;
#14157 = EDGE_LOOP ( 'NONE', ( #9650, #12257, #14170, #8024 ) ) ;
#14158 = CARTESIAN_POINT ( 'NONE',  ( 4.243569643750000786, -24.54553994094216307, -10.77318387364461572 ) ) ;
#14159 = CARTESIAN_POINT ( 'NONE',  ( -3.607379964056306676, 30.24680007765647360, 2.690724712371306282 ) ) ;
#14160 = AXIS2_PLACEMENT_3D ( 'NONE', #4574, #4388, #5694 ) ;
#14161 = VERTEX_POINT ( 'NONE', #9295 ) ;
#14162 = COLOUR_RGB ( '',0.8941176470588234615, 0.8941176470588234615, 0.8941176470588234615 ) ;
#14163 = DIRECTION ( 'NONE',  ( 0.000000000000000000, 0.000000000000000000, 1.000000000000000000 ) ) ;
#14164 = CIRCLE ( 'NONE', #4092, 6.500000000000000000 ) ;
#14165 = LINE ( 'NONE', #1206, #6773 ) ;
#14166 = DIRECTION ( 'NONE',  ( 1.000000000000000000, 0.000000000000000000, 0.000000000000000000 ) ) ;
#14167 = DIRECTION ( 'NONE',  ( 1.000000000000000000, 0.000000000000000000, 0.000000000000000000 ) ) ;
#14168 = CARTESIAN_POINT ( 'NONE',  ( -2.000000000000005773, -23.42011117034160605, -3.126428157563360344 ) ) ;
#14169 = CARTESIAN_POINT ( 'NONE',  ( -2.121784821875005722, -24.80278884970919506, -4.733338222474753998 ) ) ;
#14170 = ORIENTED_EDGE ( 'NONE', *, *, #5783, .T. ) ;
#14171 = DIRECTION ( 'NONE',  ( -0.000000000000000000, -1.000000000000000000, -0.000000000000000000 ) ) ;
#14172 = ORIENTED_EDGE ( 'NONE', *, *, #11576, .F. ) ;
#14173 = CARTESIAN_POINT ( 'NONE',  ( -4.000000000000004441, -26.94813206802970740, -10.17812312388048746 ) ) ;
#14174 = CARTESIAN_POINT ( 'NONE',  ( 4.898587196589413815E-16, 2.700915433685006750, 35.11257424290206330 ) ) ;
#14175 = SURFACE_SIDE_STYLE ('',( #9722 ) ) ;
#14176 = AXIS2_PLACEMENT_3D ( 'NONE', #7567, #10629, #3589 ) ;
#14177 = CARTESIAN_POINT ( 'NONE',  ( -2.733110507866328476, 17.37819992234354416, -3.862833514489096398 ) ) ;
#14178 = CARTESIAN_POINT ( 'NONE',  ( 2.115076519116425580, 26.12819992234354771, 3.012182706137062294 ) ) ;
#14179 = CARTESIAN_POINT ( 'NONE',  ( -3.999999999999997335, -23.98197726361007298, -13.99465086641710698 ) ) ;
#14180 = CARTESIAN_POINT ( 'NONE',  ( -2.481649420246374138, 37.87180007765647360, 0.8687765177876256573 ) ) ;
#14181 = EDGE_CURVE ( 'NONE', #6360, #3748, #4824, .T. ) ;
#14182 = ADVANCED_FACE ( 'NONE', ( #16734 ), #18334, .T. ) ;
#14183 = CARTESIAN_POINT ( 'NONE',  ( -2.733110507866328476, 34.87819992234354771, -3.862833514489096398 ) ) ;
#14184 = EDGE_CURVE ( 'NONE', #17065, #17116, #4110, .T. ) ;
#14185 = CARTESIAN_POINT ( 'NONE',  ( -4.000000000000004441, -25.85116713280339695, -8.611494838171019239 ) ) ;
#14186 =( BOUNDED_CURVE ( )  B_SPLINE_CURVE ( 2, ( #12754, #8393, #8475, #4313, #18077, #13879, #11264, #14054, #16953 ),
 .UNSPECIFIED., .F., .T. ) 
 B_SPLINE_CURVE_WITH_KNOTS ( ( 3, 2, 2, 2, 3 ),
 ( 0.4568965517241379559, 0.4597701149425287293, 0.4655172413793103314, 0.4712643678160919336, 0.4741379310344827624 ),
 .UNSPECIFIED. ) 
 CURVE ( )  GEOMETRIC_REPRESENTATION_ITEM ( )  RATIONAL_B_SPLINE_CURVE ( ( 0.9330127018922194093, 0.9330127018922200755, 1.000000000000000000, 0.8660254037844387076, 1.000000000000000000, 0.8660254037844387076, 1.000000000000000000, 0.9330127018922187432, 0.9330127018922194093 ) ) 
 REPRESENTATION_ITEM ( '' )  );
#14187 = EDGE_LOOP ( 'NONE', ( #8526, #8111 ) ) ;
#14188 = DIRECTION ( 'NONE',  ( 0.000000000000000000, 0.8191520442889952403, -0.5735764363510413855 ) ) ;
#14189 = CARTESIAN_POINT ( 'NONE',  ( -2.115076519116362519, 25.12180007765647360, 3.012182706137107147 ) ) ;
#14190 = CARTESIAN_POINT ( 'NONE',  ( 9.852650557354193595, -9.939667866509505956, 9.673467103803176315 ) ) ;
#14191 = CIRCLE ( 'NONE', #3830, 0.9999999999999991118 ) ;
#14192 = CARTESIAN_POINT ( 'NONE',  ( -4.243569643750004339, -25.07910933890011052, -7.263709834155468670 ) ) ;
#14193 = CARTESIAN_POINT ( 'NONE',  ( -3.673772985318219053, 23.24680007765647716, -2.599342558260952174 ) ) ;
#14194 = CARTESIAN_POINT ( 'NONE',  ( -3.999999999999997335, -18.04546114737679829, -5.516427208026009943 ) ) ;
#14195 = DIRECTION ( 'NONE',  ( 3.469446951953612217E-16, -0.000000000000000000, 1.000000000000000000 ) ) ;
#14196 = ORIENTED_EDGE ( 'NONE', *, *, #2416, .F. ) ;
#14197 = VERTEX_POINT ( 'NONE', #8176 ) ;
#14198 = CARTESIAN_POINT ( 'NONE',  ( -2.211161402132902243, 25.87180007765647360, -2.942372952327172886 ) ) ;
#14199 = CARTESIAN_POINT ( 'NONE',  ( -8.999999999999994671, -10.00000000000000178, 15.14468620625657103 ) ) ;
#14200 = PRESENTATION_STYLE_ASSIGNMENT (( #8529 ) ) ;
#14201 = CARTESIAN_POINT ( 'NONE',  ( 4.898587196589413815E-16, 33.00000000000000000, 4.000000000000000888 ) ) ;
#14202 = CARTESIAN_POINT ( 'NONE',  ( -5.577813053751546416E-15, -26.22509622848567545, -6.198051655426662698 ) ) ;
#14203 = ORIENTED_EDGE ( 'NONE', *, *, #6152, .F. ) ;
#14204 = CARTESIAN_POINT ( 'NONE',  ( 2.798362969681409851, 16.00319992234354416, 2.102939460078764977 ) ) ;
#14205 = CARTESIAN_POINT ( 'NONE',  ( -2.121784821874996396, -19.61005822318693248, -10.13182066358236888 ) ) ;
#14206 = CARTESIAN_POINT ( 'NONE',  ( 0.05938372350926800214, 17.37180007765647716, 2.628655560595669183 ) ) ;
#14207 = AXIS2_PLACEMENT_3D ( 'NONE', #12495, #3885, #18189 ) ;
#14208 = VECTOR ( 'NONE', #6064, 1000.000000000000000 ) ;
#14209 = CARTESIAN_POINT ( 'NONE',  ( -2.115076519116425580, 34.87819992234354771, -3.012182706137062738 ) ) ;
#14210 = DIRECTION ( 'NONE',  ( -0.000000000000000000, 0.000000000000000000, -1.000000000000000000 ) ) ;
#14211 = EDGE_CURVE ( 'NONE', #15334, #14506, #12963, .T. ) ;
#14212 = CARTESIAN_POINT ( 'NONE',  ( 4.000000000000000888, -24.94883587310395967, -11.34915015528869731 ) ) ;
#14213 = CARTESIAN_POINT ( 'NONE',  ( -4.243569643750005227, -24.59515422072892221, -6.572550296786629609 ) ) ;
#14214 = MANIFOLD_SOLID_BREP ( 'LPattern6[10]', #13845 ) ;
#14215 = CIRCLE ( 'NONE', #10954, 4.000000000000000000 ) ;
#14216 = DIRECTION ( 'NONE',  ( 0.000000000000000000, -0.000000000000000000, -1.000000000000000000 ) ) ;
#14217 = CIRCLE ( 'NONE', #13031, 10.00000000000000000 ) ;
#14218 = DIRECTION ( 'NONE',  ( -1.000000000000000000, -0.000000000000000000, -0.000000000000000000 ) ) ;
#14219 = CARTESIAN_POINT ( 'NONE',  ( -1.999999999999996225, -18.15353254261686899, -7.683928109263233885 ) ) ;
#14220 = CARTESIAN_POINT ( 'NONE',  ( 4.243569643749996345, -22.67008830622574322, -3.823271248141685508 ) ) ;
#14221 = CARTESIAN_POINT ( 'NONE',  ( -2.987022202050954700, 15.00000000000010125, -0.3375100304031865561 ) ) ;
#14222 = DIRECTION ( 'NONE',  ( 0.000000000000000000, 0.000000000000000000, -1.000000000000000000 ) ) ;
#14223 = ORIENTED_EDGE ( 'NONE', *, *, #8513, .T. ) ;
#14224 = ADVANCED_FACE ( 'NONE', ( #17091 ), #12080, .T. ) ;
#14225 = CARTESIAN_POINT ( 'NONE',  ( -0.7188294034286550893, 22.50319992234354771, -2.395093729190349130 ) ) ;
#14226 = FACE_OUTER_BOUND ( 'NONE', #4177, .T. ) ;
#14227 = CARTESIAN_POINT ( 'NONE',  ( 1.027846397803542144, 18.74680007765648071, -3.346150245485522312 ) ) ;
#14228 = DIRECTION ( 'NONE',  ( 0.000000000000000000, 0.000000000000000000, -1.000000000000000000 ) ) ;
#14229 = DIRECTION ( 'NONE',  ( 0.000000000000000000, 0.000000000000000000, -1.000000000000000000 ) ) ;
#14230 = ORIENTED_EDGE ( 'NONE', *, *, #18063, .T. ) ;
#14231 = CARTESIAN_POINT ( 'NONE',  ( -4.243569643749998122, -18.30130014856414533, -6.126975372181462376 ) ) ;
#14232 = CIRCLE ( 'NONE', #7703, 0.9999999999999991118 ) ;
#14233 = CARTESIAN_POINT ( 'NONE',  ( -1.135272562821090014, 35.99680007765648071, -3.311245368580554072 ) ) ;
#14234 = CARTESIAN_POINT ( 'NONE',  ( 1.999999999999994449, -22.60276474854137874, -1.959136494451539035 ) ) ;
#14235 = APPLICATION_CONTEXT ( 'automotive_design' ) ;
#14236 = CARTESIAN_POINT ( 'NONE',  ( -5.330712181944246111E-15, -29.10791014587222847, -8.745943564552382199 ) ) ;
#14237 = CARTESIAN_POINT ( 'NONE',  ( 0.000000000000000000, 23.19999999999999574, 2.500000000000000000 ) ) ;
#14238 = CARTESIAN_POINT ( 'NONE',  ( 19.30950000000002120, 4.898587196589414801E-16, -4.000000000000000888 ) ) ;
#14239 = CARTESIAN_POINT ( 'NONE',  ( -1.734723475976807094E-15, 18.79999999999999361, -2.500000000000000000 ) ) ;
#14240 = CARTESIAN_POINT ( 'NONE',  ( 2.121784821875004390, -21.71795162677701896, -13.14220442634442243 ) ) ;
#14241 = CYLINDRICAL_SURFACE ( 'NONE', #5939, 2.000000000000000000 ) ;
#14242 = CARTESIAN_POINT ( 'NONE',  ( -1.999999999999996225, -16.86298556082702760, -5.840836009612994317 ) ) ;
#14243 = CIRCLE ( 'NONE', #6235, 5.000000000000000000 ) ;
#14244 = CARTESIAN_POINT ( 'NONE',  ( 2.518350579753628971, 19.37180007765648071, 0.7558219633769073242 ) ) ;
#14245 = ORIENTED_EDGE ( 'NONE', *, *, #12728, .T. ) ;
#14246 = CARTESIAN_POINT ( 'NONE',  ( 1.027846397803542144, 21.24680007765647716, -3.346150245485522312 ) ) ;
#14247 = CARTESIAN_POINT ( 'NONE',  ( 2.856226148085021954, -24.67072674863668169, -15.86966854801251081 ) ) ;
#14248 = EDGE_CURVE ( 'NONE', #10194, #278, #10013, .T. ) ;
#14249 = DIRECTION ( 'NONE',  ( -0.000000000000000000, -0.5735764363510414965, -0.8191520442889950182 ) ) ;
#14250 = CARTESIAN_POINT ( 'NONE',  ( -2.481649420246391902, 32.12819992234354771, -0.8687765177875723666 ) ) ;
#14251 = ADVANCED_FACE ( 'NONE', ( #4011 ), #9654, .F. ) ;
#14252 = EDGE_LOOP ( 'NONE', ( #5895, #6513, #2697, #17240, #13185, #13470 ) ) ;
#14253 = CARTESIAN_POINT ( 'NONE',  ( 4.730628863548789710E-15, -19.69279666510938043, -12.38572846031554953 ) ) ;
#14254 = CARTESIAN_POINT ( 'NONE',  ( -0.05938372350928957516, 33.62180007765647360, -4.731580009072201776 ) ) ;
#14255 = EDGE_CURVE ( 'NONE', #10347, #17611, #16847, .T. ) ;
#14256 = VERTEX_POINT ( 'NONE', #1331 ) ;
#14257 = MECHANICAL_DESIGN_GEOMETRIC_PRESENTATION_REPRESENTATION (  '', ( #42 ), #15158 ) ;
#14258 = PRESENTATION_STYLE_ASSIGNMENT (( #5636 ) ) ;
#14259 = CARTESIAN_POINT ( 'NONE',  ( 4.299564228933482956E-15, -19.28471577963676964, -10.23373551633992307 ) ) ;
#14260 = CARTESIAN_POINT ( 'NONE',  ( -8.500000000000005329, 10.00000000000000000, 20.49999999999999645 ) ) ;
#14261 = DIRECTION ( 'NONE',  ( -1.000000000000000000, -0.000000000000000000, -0.000000000000000000 ) ) ;
#14262 = CARTESIAN_POINT ( 'NONE',  ( -1.661723472263481630E-14, -21.28506360070608139, -13.09052826979102946 ) ) ;
#14263 = CARTESIAN_POINT ( 'NONE',  ( -4.243569643750000786, -20.80295369375161130, -5.428216784658927985 ) ) ;
#14264 = ORIENTED_EDGE ( 'NONE', *, *, #2652, .F. ) ;
#14265 = FACE_OUTER_BOUND ( 'NONE', #2134, .T. ) ;
#14266 = VERTEX_POINT ( 'NONE', #8617 ) ;
#14267 = EDGE_LOOP ( 'NONE', ( #9356, #16631, #5467, #11054 ) ) ;
#14268 = CARTESIAN_POINT ( 'NONE',  ( -2.000000000000005773, -23.22652912377807510, -2.849964343622590324 ) ) ;
#14269 =( NAMED_UNIT ( * ) SI_UNIT ( $, .STERADIAN. ) SOLID_ANGLE_UNIT ( ) );
#14270 = PRESENTATION_LAYER_ASSIGNMENT (  '', '', ( #11896 ) ) ;
#14271 = CARTESIAN_POINT ( 'NONE',  ( 0.05938372350919016857, 17.62819992234354416, -4.731580009072201776 ) ) ;
#14272 = CARTESIAN_POINT ( 'NONE',  ( 2.115076519116425580, 28.62819992234354061, 3.012182706137062294 ) ) ;
#14273 = CARTESIAN_POINT ( 'NONE',  ( 0.7188294034286049072, 36.24680007765647360, -2.395093729190366005 ) ) ;
#14274 = MANIFOLD_SOLID_BREP ( 'Boss-Extrude2', #7631 ) ;
#14275 = VERTEX_POINT ( 'NONE', #14679 ) ;
#14276 = CARTESIAN_POINT ( 'NONE',  ( -4.499999999999999112, 34.50319992234354771, -0.05647727720528529505 ) ) ;
#14277 = CARTESIAN_POINT ( 'NONE',  ( 2.000000000000004441, -20.19689859641251317, -10.60215726603601283 ) ) ;
#14278 = EDGE_LOOP ( 'NONE', ( #17352, #10098, #8146, #13696 ) ) ;
#14279 = AXIS2_PLACEMENT_3D ( 'NONE', #4318, #13029, #14153 ) ;
#14280 = DIRECTION ( 'NONE',  ( -0.000000000000000000, -1.000000000000000000, -0.000000000000000000 ) ) ;
#14281 = PRESENTATION_LAYER_ASSIGNMENT (  '', '', ( #2168 ) ) ;
#14282 = CARTESIAN_POINT ( 'NONE',  ( 3.481649420246369697, 29.12180007765647005, -1.193696214020541824 ) ) ;
#14283 = DIRECTION ( 'NONE',  ( -1.000000000000000000, 0.000000000000000000, 4.336808689942021680E-16 ) ) ;
#14284 = AXIS2_PLACEMENT_3D ( 'NONE', #17421, #5802, #17330 ) ;
#14285 = CARTESIAN_POINT ( 'NONE',  ( 4.243569643750000786, -22.44840109553366858, -7.778159211712977417 ) ) ;
#14286 = CARTESIAN_POINT ( 'NONE',  ( 3.673772985318219053, 34.49680007765647360, 2.599342558260951730 ) ) ;
#14287 = DIRECTION ( 'NONE',  ( -0.000000000000000000, 0.000000000000000000, 1.000000000000000000 ) ) ;
#14288 = ORIENTED_EDGE ( 'NONE', *, *, #2967, .T. ) ;
#14289 = ORIENTED_EDGE ( 'NONE', *, *, #6934, .T. ) ;
#14290 = CARTESIAN_POINT ( 'NONE',  ( -2.115076519116362519, 22.62180007765647360, 3.012182706137107147 ) ) ;
#14291 = EDGE_CURVE ( 'NONE', #11559, #6787, #16100, .T. ) ;
#14292 = DIRECTION ( 'NONE',  ( -3.469446951953613696E-16, -0.000000000000000000, -1.000000000000000000 ) ) ;
#14293 = AXIS2_PLACEMENT_3D ( 'NONE', #14340, #11540, #15640 ) ;
#14294 = CARTESIAN_POINT ( 'NONE',  ( -1.071796769724505882, -18.24075149348606573, -8.742800001963811241 ) ) ;
#14295 =( LENGTH_UNIT ( ) NAMED_UNIT ( * ) SI_UNIT ( .MILLI., .METRE. ) );
#14296 = ORIENTED_EDGE ( 'NONE', *, *, #18289, .T. ) ;
#14297 = CARTESIAN_POINT ( 'NONE',  ( -2.864755990943222308, 19.25319992234354416, 2.011557305968548093 ) ) ;
#14298 = CARTESIAN_POINT ( 'NONE',  ( 2.121784821874994176, -25.24372573515406515, -5.363061356521914291 ) ) ;
#14299 = CARTESIAN_POINT ( 'NONE',  ( 3.500000000000000444, 39.24680007765647360, -0.05647727720536935281 ) ) ;
#14300 =( BOUNDED_CURVE ( )  B_SPLINE_CURVE ( 2, ( #3593, #13595, #9243, #12111, #17982, #10723, #16400, #3685, #15008 ),
 .UNSPECIFIED., .F., .T. ) 
 B_SPLINE_CURVE_WITH_KNOTS ( ( 3, 2, 2, 2, 3 ),
 ( 0.3362068965517241437, 0.3390804597701149170, 0.3448275862068965747, 0.3505747126436781769, 0.3534482758620690057 ),
 .UNSPECIFIED. ) 
 CURVE ( )  GEOMETRIC_REPRESENTATION_ITEM ( )  RATIONAL_B_SPLINE_CURVE ( ( 0.9330127018922194093, 0.9330127018922200755, 1.000000000000000000, 0.8660254037844387076, 1.000000000000000000, 0.8660254037844387076, 1.000000000000000000, 0.9330127018922187432, 0.9330127018922194093 ) ) 
 REPRESENTATION_ITEM ( '' )  );
#14301 = CARTESIAN_POINT ( 'NONE',  ( 1.027846397803612311, 38.75319992234354061, 3.346150245485499219 ) ) ;
#14302 = CARTESIAN_POINT ( 'NONE',  ( 1.300000000000000044, -1.443375672974064328, 2.168404344971008868E-16 ) ) ;
#14303 = CARTESIAN_POINT ( 'NONE',  ( 0.000000000000000000, 5.977523610840987267, 32.81826849749789687 ) ) ;
#14304 = CARTESIAN_POINT ( 'NONE',  ( -2.121784821875005722, -26.35144522785700616, -6.945048742055040414 ) ) ;
#14305 = MANIFOLD_SOLID_BREP ( 'Cavity1', #539 ) ;
#14306 = VECTOR ( 'NONE', #2410, 1000.000000000000000 ) ;
#14307 = TOROIDAL_SURFACE ( 'NONE', #9277, 9.000000000000001776, 0.9999999999999991118 ) ;
#14308 = CARTESIAN_POINT ( 'NONE',  ( 0.5553297335976642435, -10.00000000000086686, -4.810349131761211261 ) ) ;
#14309 = EDGE_CURVE ( 'NONE', #14256, #13681, #1625, .T. ) ;
#14310 = FACE_OUTER_BOUND ( 'NONE', #12026, .T. ) ;
#14311 = EDGE_CURVE ( 'NONE', #7786, #1402, #8834, .T. ) ;
#14312 = CARTESIAN_POINT ( 'NONE',  ( -4.000000000000000888, -24.75525382513053430, -11.07268633933439972 ) ) ;
#14313 = CARTESIAN_POINT ( 'NONE',  ( -2.121784821875005722, -23.22186879701663642, -2.475550400403212503 ) ) ;
#14314 = DIRECTION ( 'NONE',  ( 3.469446951953612217E-16, -0.000000000000000000, 1.000000000000000000 ) ) ;
#14315 = SURFACE_STYLE_USAGE ( .BOTH. , #16934 ) ;
#14316 = EDGE_CURVE ( 'NONE', #14997, #14652, #3227, .T. ) ;
#14317 = EDGE_LOOP ( 'NONE', ( #8919, #2538, #11375, #7248, #13549 ) ) ;
#14318 = CARTESIAN_POINT ( 'NONE',  ( -1.989345975306457071, 17.25319992234354416, -1.515154207786300944 ) ) ;
#14319 = CARTESIAN_POINT ( 'NONE',  ( 4.243569643750000786, -26.83626083361913217, -14.04467235052378804 ) ) ;
#14320 = CARTESIAN_POINT ( 'NONE',  ( -1.135272562821090014, 15.99680007765647716, -3.311245368580554072 ) ) ;
#14321 = VECTOR ( 'NONE', #16388, 1000.000000000000000 ) ;
#14322 = CARTESIAN_POINT ( 'NONE',  ( 4.000000000000000000, -1.759474945355381292, 3.047500000000002540 ) ) ;
#14323 = FACE_OUTER_BOUND ( 'NONE', #7645, .T. ) ;
#14324 = ORIENTED_EDGE ( 'NONE', *, *, #16762, .T. ) ;
#14325 = CARTESIAN_POINT ( 'NONE',  ( -4.243569643749998122, -18.04319075220617563, -5.758356952251413752 ) ) ;
#14326 = CARTESIAN_POINT ( 'NONE',  ( -3.518350579753630747, 35.62180007765648782, -1.080741659609802729 ) ) ;
#14327 = CARTESIAN_POINT ( 'NONE',  ( -4.243569643750000786, -26.48136041362692339, -13.53782202311997551 ) ) ;
#14328 = SURFACE_STYLE_USAGE ( .BOTH. , #6988 ) ;
#14329 = CARTESIAN_POINT ( 'NONE',  ( -5.330712181944246111E-15, -29.88223833494613402, -9.851798824342527183 ) ) ;
#14330 = CARTESIAN_POINT ( 'NONE',  ( 0.000000000000000000, 33.00000000000000000, 0.000000000000000000 ) ) ;
#14331 = VECTOR ( 'NONE', #7629, 1000.000000000000000 ) ;
#14332 = DIRECTION ( 'NONE',  ( 0.000000000000000000, 0.000000000000000000, 1.000000000000000000 ) ) ;
#14333 = DIRECTION ( 'NONE',  ( -1.000000000000000000, 0.000000000000000000, -0.000000000000000000 ) ) ;
#14334 = CARTESIAN_POINT ( 'NONE',  ( -4.243569643749997233, -22.65689621210486138, -12.34741120850101836 ) ) ;
#14335 = CARTESIAN_POINT ( 'NONE',  ( 0.000000000000000000, 5.977523610840987267, 32.81826849749789687 ) ) ;
#14336 = CARTESIAN_POINT ( 'NONE',  ( 4.000000000000003553, -19.16393519826133485, -7.113773694389545099 ) ) ;
#14337 = CARTESIAN_POINT ( 'NONE',  ( 2.500000000000001332, 21.74680007765648071, -0.05647727720535888202 ) ) ;
#14338 = EDGE_LOOP ( 'NONE', ( #12283, #762, #7542, #4357, #12333, #16417, #14104, #7302, #14726 ) ) ;
#14339 = CARTESIAN_POINT ( 'NONE',  ( 2.798362969681366330, 18.99680007765648071, -2.102939460078824929 ) ) ;
#14340 = CARTESIAN_POINT ( 'NONE',  ( 0.000000000000000000, 5.977523610840987267, 32.81826849749789687 ) ) ;
#14341 =( NAMED_UNIT ( * ) SI_UNIT ( $, .STERADIAN. ) SOLID_ANGLE_UNIT ( ) );
#14342 = CARTESIAN_POINT ( 'NONE',  ( 4.000000000000003553, -21.42239241568860564, -10.33918486777069745 ) ) ;
#14343 = CARTESIAN_POINT ( 'NONE',  ( 2.500000000000001332, 38.25319992234354771, 0.05647727720530566764 ) ) ;
#14344 = EDGE_LOOP ( 'NONE', ( #2628, #8896, #15151, #12326 ) ) ;
#14345 = CARTESIAN_POINT ( 'NONE',  ( 4.243569643750003451, -22.25897755938633793, -11.77912447777552174 ) ) ;
#14346 = CARTESIAN_POINT ( 'NONE',  ( -1.444289557196047014, 33.49680007765648071, -4.262301884875704161 ) ) ;
#14347 = EDGE_LOOP ( 'NONE', ( #4905, #1760, #18218, #18174 ) ) ;
#14348 = DIRECTION ( 'NONE',  ( 0.000000000000000000, 0.000000000000000000, 1.000000000000000000 ) ) ;
#14349 = CARTESIAN_POINT ( 'NONE',  ( 3.999999999999996447, -24.73269308191887461, -7.014148351807473425 ) ) ;
#14350 = CARTESIAN_POINT ( 'NONE',  ( 2.121784821875004390, -22.26643409403770590, -13.92551856869577342 ) ) ;
#14351 = DIRECTION ( 'NONE',  ( 0.000000000000000000, 0.8660254037844385966, -0.5000000000000003331 ) ) ;
#14352 = PLANE ( 'NONE',  #4727 ) ;
#14353 = DIRECTION ( 'NONE',  ( -1.000000000000000000, -0.000000000000000000, -0.000000000000000000 ) ) ;
#14354 = CARTESIAN_POINT ( 'NONE',  ( 2.121784821874994176, -23.72733303155099804, -3.197428139432884286 ) ) ;
#14355 = EDGE_CURVE ( 'NONE', #17116, #17908, #1040, .T. ) ;
#14356 = ORIENTED_EDGE ( 'NONE', *, *, #13200, .T. ) ;
#14357 = CARTESIAN_POINT ( 'NONE',  ( 2.000000000000004441, -20.19689859641251317, -10.60215726603601283 ) ) ;
#14358 = ORIENTED_EDGE ( 'NONE', *, *, #14897, .F. ) ;
#14359 = ORIENTED_EDGE ( 'NONE', *, *, #16511, .F. ) ;
#14360 = DIRECTION ( 'NONE',  ( 0.000000000000000000, 0.000000000000000000, -1.000000000000000000 ) ) ;
#14361 = ADVANCED_FACE ( 'NONE', ( #850 ), #12394, .T. ) ;
#14362 = CARTESIAN_POINT ( 'NONE',  ( 8.500000000000019540, 10.00000000000000000, -20.49999999999998934 ) ) ;
#14363 = PRESENTATION_STYLE_ASSIGNMENT (( #13239 ) ) ;
#14364 = CARTESIAN_POINT ( 'NONE',  ( -3.518350579753605434, 39.37819992234354771, 1.080741659609877781 ) ) ;
#14365 = CARTESIAN_POINT ( 'NONE',  ( -1.027846397803611866, 25.00319992234354416, -3.346150245485499219 ) ) ;
#14366 = CARTESIAN_POINT ( 'NONE',  ( -2.055738996568313048, 35.74680007765648071, -1.423772053676023441 ) ) ;
#14367 = ORIENTED_EDGE ( 'NONE', *, *, #6992, .F. ) ;
#14368 = CARTESIAN_POINT ( 'NONE',  ( 1.336863392178569754, 31.25319992234354416, 4.297206761780648421 ) ) ;
#14369 = CARTESIAN_POINT ( 'NONE',  ( 1.999999999999994449, -26.73251509026887618, -7.857031213332303921 ) ) ;
#14370 = ORIENTED_EDGE ( 'NONE', *, *, #9824, .T. ) ;
#14371 = CARTESIAN_POINT ( 'NONE',  ( -1.734723475976807094E-15, 34.19999999999999574, -11.50000000000000178 ) ) ;
#14372 = CARTESIAN_POINT ( 'NONE',  ( -2.864755990943265829, 33.24680007765648071, -2.011557305968488141 ) ) ;
#14373 = CARTESIAN_POINT ( 'NONE',  ( 3.999999999999996447, 6.938893903907228378E-15, 24.28148006742132026 ) ) ;
#14374 = CARTESIAN_POINT ( 'NONE',  ( 2.121784821875004390, -18.36252947412342351, -8.350164967253801862 ) ) ;
#14375 = CARTESIAN_POINT ( 'NONE',  ( 2.733110507866247652, 28.87180007765647716, -3.862833514489153686 ) ) ;
#14376 = CARTESIAN_POINT ( 'NONE',  ( -1.734723475976807094E-15, 16.59999999999999787, -11.50000000000000178 ) ) ;
#14377 = EDGE_CURVE ( 'NONE', #1806, #15033, #9204, .T. ) ;
#14378 = ORIENTED_EDGE ( 'NONE', *, *, #5322, .T. ) ;
#14379 = ORIENTED_EDGE ( 'NONE', *, *, #8295, .T. ) ;
#14380 = CARTESIAN_POINT ( 'NONE',  ( -1.027846397803541700, 19.99680007765648071, 3.346150245485522312 ) ) ;
#14381 = DIRECTION ( 'NONE',  ( -1.000000000000000000, 0.000000000000000000, 4.336808689942021680E-16 ) ) ;
#14382 = DIRECTION ( 'NONE',  ( -0.000000000000000000, -0.5000000000000002220, -0.8660254037844384856 ) ) ;
#14383 = CARTESIAN_POINT ( 'NONE',  ( -1.734723475976807094E-15, 29.79999999999999716, -12.50000000000000000 ) ) ;
#14384 = ORIENTED_EDGE ( 'NONE', *, *, #15852, .T. ) ;
#14385 = CARTESIAN_POINT ( 'NONE',  ( -3.481649420246394122, 17.12819992234354061, -1.193696214020467883 ) ) ;
#14386 = FACE_OUTER_BOUND ( 'NONE', #2055, .T. ) ;
#14387 = CARTESIAN_POINT ( 'NONE',  ( 4.243569643750003451, -21.19427629940971869, -10.25857349556407527 ) ) ;
#14388 = CARTESIAN_POINT ( 'NONE',  ( 3.518350579753631191, 39.37180007765646650, 1.080741659609802285 ) ) ;
#14389 = CARTESIAN_POINT ( 'NONE',  ( -1.135272562821019626, 34.00319992234354771, 3.311245368580577164 ) ) ;
#14390 = FACE_OUTER_BOUND ( 'NONE', #7775, .T. ) ;
#14391 = CARTESIAN_POINT ( 'NONE',  ( -1.999999999999996225, -24.28363070541367819, -16.43861558159510494 ) ) ;
#14392 = AXIS2_PLACEMENT_3D ( 'NONE', #3835, #12629, #18045 ) ;
#14393 = CARTESIAN_POINT ( 'NONE',  ( -4.243569643750005227, -24.33704482437095251, -6.203931876856584537 ) ) ;
#14394 = CIRCLE ( 'NONE', #8449, 8.000000000000003553 ) ;
#14395 = CARTESIAN_POINT ( 'NONE',  ( -10.00000000000000000, 18.79999999999999361, 2.499999999999996003 ) ) ;
#14396 = CARTESIAN_POINT ( 'NONE',  ( -5.940121053391560935, -10.00000000000000178, -9.400027718825146650 ) ) ;
#14397 = DIRECTION ( 'NONE',  ( -1.000000000000000000, 0.000000000000000000, 0.000000000000000000 ) ) ;
#14398 = CARTESIAN_POINT ( 'NONE',  ( 8.000000000000005329, 23.19999999999999574, 2.499999999999997780 ) ) ;
#14399 =( BOUNDED_CURVE ( )  B_SPLINE_CURVE ( 2, ( #2221, #14929, #7848, #16675, #12292, #12387, #816, #17713, #6553 ),
 .UNSPECIFIED., .F., .T. ) 
 B_SPLINE_CURVE_WITH_KNOTS ( ( 3, 2, 2, 2, 3 ),
 ( 0.6982758620689655249, 0.7011494252873563537, 0.7068965517241379004, 0.7126436781609195581, 0.7155172413793103869 ),
 .UNSPECIFIED. ) 
 CURVE ( )  GEOMETRIC_REPRESENTATION_ITEM ( )  RATIONAL_B_SPLINE_CURVE ( ( 0.9330127018922194093, 0.9330127018922194093, 1.000000000000000000, 0.8660254037844387076, 1.000000000000000000, 0.8660254037844387076, 1.000000000000000000, 0.9330127018922180770, 0.9330127018922194093 ) ) 
 REPRESENTATION_ITEM ( '' )  );
#14400 = CARTESIAN_POINT ( 'NONE',  ( -2.121784821875005722, -23.47997819337460257, -2.844168820333258907 ) ) ;
#14401 = CARTESIAN_POINT ( 'NONE',  ( -1.514047762142602060, 14.99999999999999645, -2.869914431049744863 ) ) ;
#14402 = DIRECTION ( 'NONE',  ( 0.000000000000000000, 0.000000000000000000, -1.000000000000000000 ) ) ;
#14403 = ORIENTED_EDGE ( 'NONE', *, *, #17630, .T. ) ;
#14404 = CARTESIAN_POINT ( 'NONE',  ( 2.518350579753611207, 23.12819992234354416, -0.7558219633769606149 ) ) ;
#14405 = AXIS2_PLACEMENT_3D ( 'NONE', #15543, #18251, #51 ) ;
#14406 = CARTESIAN_POINT ( 'NONE',  ( -2.121784821874996396, -23.73980856491443703, -16.02971538246313443 ) ) ;
#14407 = CARTESIAN_POINT ( 'NONE',  ( 9.000000000000000000, 31.99999999999999289, -2.500000000000001332 ) ) ;
#14408 = CARTESIAN_POINT ( 'NONE',  ( -3.673772985318163098, 39.25319992234354771, 2.599342558261029001 ) ) ;
#14409 = CARTESIAN_POINT ( 'NONE',  ( 9.999999999999998224, 23.19999999999999574, -2.500000000000001776 ) ) ;
#14410 = DIRECTION ( 'NONE',  ( 0.000000000000000000, 0.000000000000000000, 1.000000000000000000 ) ) ;
#14411 = EDGE_CURVE ( 'NONE', #10626, #12954, #411, .T. ) ;
#14412 = ORIENTED_EDGE ( 'NONE', *, *, #6327, .T. ) ;
#14413 = CARTESIAN_POINT ( 'NONE',  ( 4.730628863548789710E-15, -16.07926511609781883, -7.225070581294880334 ) ) ;
#14414 = CARTESIAN_POINT ( 'NONE',  ( -2.798362969681365886, 37.74680007765647360, 2.102939460078824929 ) ) ;
#14415 = CARTESIAN_POINT ( 'NONE',  ( -2.121784821875005722, -29.44875798415262835, -11.36846978121561236 ) ) ;
#14416 = EDGE_CURVE ( 'NONE', #1959, #7464, #6049, .T. ) ;
#14417 = EDGE_CURVE ( 'NONE', #18202, #15889, #14782, .T. ) ;
#14418 = LINE ( 'NONE', #12244, #11988 ) ;
#14419 = TOROIDAL_SURFACE ( 'NONE', #14729, 9.000000000000001776, 0.9999999999999991118 ) ;
#14420 = CARTESIAN_POINT ( 'NONE',  ( 2.121784821875004390, -23.00849860856686036, -14.98529652599465933 ) ) ;
#14421 = CARTESIAN_POINT ( 'NONE',  ( -3.706921591972381904E-14, -16.70362181605707619, -6.547551317039444818 ) ) ;
#14422 = EDGE_CURVE ( 'NONE', #16136, #12954, #17143, .T. ) ;
#14423 = CARTESIAN_POINT ( 'NONE',  ( -9.000000000000001776, 31.99999999999999289, 2.499999999999998224 ) ) ;
#14424 = CARTESIAN_POINT ( 'NONE',  ( -8.500000000000010658, 14.80000000000000071, 20.49999999999998934 ) ) ;
#14425 = CARTESIAN_POINT ( 'NONE',  ( 2.121784821875004390, -21.20173283406107956, -12.40496758648432518 ) ) ;
#14426 = DIRECTION ( 'NONE',  ( 0.000000000000000000, 0.000000000000000000, -1.000000000000000000 ) ) ;
#14427 = CARTESIAN_POINT ( 'NONE',  ( -2.000000000000005773, -23.22652912377807510, -2.849964343622590324 ) ) ;
#14428 = CARTESIAN_POINT ( 'NONE',  ( -2.500000000000001332, 25.49680007765647716, 0.05647727720535858364 ) ) ;
#14429 = ORIENTED_EDGE ( 'NONE', *, *, #8168, .F. ) ;
#14430 = CARTESIAN_POINT ( 'NONE',  ( -0.05938372350927861865, 21.12180007765647716, -3.680117784833935701 ) ) ;
#14431 = EDGE_CURVE ( 'NONE', #317, #16065, #16268, .T. ) ;
#14432 = DIRECTION ( 'NONE',  ( 0.000000000000000000, 0.000000000000000000, -1.000000000000000000 ) ) ;
#14433 = DIRECTION ( 'NONE',  ( 1.000000000000000000, 0.000000000000000000, 0.000000000000000000 ) ) ;
#14434 = CIRCLE ( 'NONE', #1750, 10.00000000000000000 ) ;
#14435 = CARTESIAN_POINT ( 'NONE',  ( 1.999999999999994449, -26.21629629755294033, -7.119794373472207560 ) ) ;
#14436 = AXIS2_PLACEMENT_3D ( 'NONE', #12839, #8306, #1631 ) ;
#14437 = CARTESIAN_POINT ( 'NONE',  ( -3.518350579753605434, 16.87819992234353705, 1.080741659609877781 ) ) ;
#14438 =( BOUNDED_CURVE ( )  B_SPLINE_CURVE ( 2, ( #5333, #2384, #2656, #13860, #1349, #6632, #10890, #9495, #11071 ),
 .UNSPECIFIED., .F., .F. ) 
 B_SPLINE_CURVE_WITH_KNOTS ( ( 3, 2, 2, 2, 3 ),
 ( 0.4741379310344827624, 0.4770114942528735358, 0.4827586206896551935, 0.4885057471264367956, 0.4913793103448276245 ),
 .UNSPECIFIED. ) 
 CURVE ( )  GEOMETRIC_REPRESENTATION_ITEM ( )  RATIONAL_B_SPLINE_CURVE ( ( 0.9330127018922194093, 0.9330127018922200755, 1.000000000000000000, 0.8660254037844387076, 1.000000000000000000, 0.8660254037844387076, 1.000000000000000000, 0.9330127018922187432, 0.9330127018922194093 ) ) 
 REPRESENTATION_ITEM ( '' )  );
#14439 = EDGE_LOOP ( 'NONE', ( #281, #17429, #10822, #1390, #6565, #1364, #4986 ) ) ;
#14440 = CARTESIAN_POINT ( 'NONE',  ( 4.243569643749997233, -26.05777413342408622, -8.661388009723561154 ) ) ;
#14441 = CARTESIAN_POINT ( 'NONE',  ( 3.607379964056306676, 33.99680007765647360, -2.690724712371305838 ) ) ;
#14442 = ORIENTED_EDGE ( 'NONE', *, *, #12488, .T. ) ;
#14443 = CARTESIAN_POINT ( 'NONE',  ( 15.00000000000000355, -10.00000000000000000, -30.00000000000000000 ) ) ;
#14444 = CLOSED_SHELL ( 'NONE', ( #3670, #14669, #9494, #17053, #5804, #9947, #14224, #5195, #18142, #2994 ) ) ;
#14445 = AXIS2_PLACEMENT_3D ( 'NONE', #4825, #841, #6482 ) ;
#14446 = CARTESIAN_POINT ( 'NONE',  ( -2.121784821875005722, -28.93253919143669251, -10.63123294135551689 ) ) ;
#14447 = DIRECTION ( 'NONE',  ( -0.000000000000000000, 1.000000000000000000, -0.000000000000000000 ) ) ;
#14448 = CIRCLE ( 'NONE', #14445, 3.000000000000001776 ) ;
#14449 = AXIS2_PLACEMENT_3D ( 'NONE', #12861, #14171, #10260 ) ;
#14450 = CARTESIAN_POINT ( 'NONE',  ( 1.300000000000000044, -1.443375672974064328, 2.168404344971008868E-16 ) ) ;
#14451 = AXIS2_PLACEMENT_3D ( 'NONE', #8791, #8603, #377 ) ;
#14453 = CARTESIAN_POINT ( 'NONE',  ( 0.000000000000000000, 31.99999999999999289, 2.500000000000000000 ) ) ;
#14452 = VECTOR ( 'NONE', #7824, 1000.000000000000227 ) ;
#14454 = CARTESIAN_POINT ( 'NONE',  ( 4.243569643750000786, -21.96444597736247673, -7.086999674344137468 ) ) ;
#14455 = ORIENTED_EDGE ( 'NONE', *, *, #1701, .F. ) ;
#14456 = FACE_OUTER_BOUND ( 'NONE', #16990, .T. ) ;
#14457 = FACE_OUTER_BOUND ( 'NONE', #7226, .T. ) ;
#14458 = ORIENTED_EDGE ( 'NONE', *, *, #14766, .T. ) ;
#14459 = EDGE_LOOP ( 'NONE', ( #9313, #1558, #180, #749 ) ) ;
#14460 = DIRECTION ( 'NONE',  ( 0.000000000000000000, -0.000000000000000000, -1.000000000000000000 ) ) ;
#14461 = LINE ( 'NONE', #1763, #16373 ) ;
#14462 = CARTESIAN_POINT ( 'NONE',  ( -3.607379964056363075, 29.75319992234354416, -2.690724712371229899 ) ) ;
#14463 = ADVANCED_FACE ( 'NONE', ( #3558, #2181 ), #777, .F. ) ;
#14464 = CARTESIAN_POINT ( 'NONE',  ( -1.135272562821019626, 26.50319992234354771, 3.311245368580577164 ) ) ;
#14465 = CARTESIAN_POINT ( 'NONE',  ( 0.7188294034286049072, 38.74680007765646650, -2.395093729190366005 ) ) ;
#14467 = MANIFOLD_SOLID_BREP ( 'Cut-Extrude2', #6449 ) ;
#14466 = CLOSED_SHELL ( 'NONE', ( #13772, #17730, #3271, #17096, #10787, #10326, #5244 ) ) ;
#14468 = EDGE_LOOP ( 'NONE', ( #9343, #10189, #6217, #11887 ) ) ;
#14469 = VECTOR ( 'NONE', #18134, 1000.000000000000000 ) ;
#14470 = CARTESIAN_POINT ( 'NONE',  ( -3.673772985318163098, 36.75319992234353350, 2.599342558261029001 ) ) ;
#14471 = VECTOR ( 'NONE', #1801, 1000.000000000000000 ) ;
#14472 = CARTESIAN_POINT ( 'NONE',  ( 4.000000000000003553, -20.64806422661470720, -9.233329607980554243 ) ) ;
#14473 = ORIENTED_EDGE ( 'NONE', *, *, #2613, .F. ) ;
#14474 = CARTESIAN_POINT ( 'NONE',  ( 1.071796769724485232, -24.14869435690309984, -3.232642461330365702 ) ) ;
#14475 = CARTESIAN_POINT ( 'NONE',  ( -1.027846397803541700, 27.49680007765648071, 3.346150245485522312 ) ) ;
#14476 = CARTESIAN_POINT ( 'NONE',  ( -5.993188111103413540, -10.31462179351540875, 0.09365451271231550745 ) ) ;
#14477 = CARTESIAN_POINT ( 'NONE',  ( 4.243569643750003451, -20.16183871397783633, -8.784099815843886105 ) ) ;
#14478 = CARTESIAN_POINT ( 'NONE',  ( -3.673772985318219053, 30.74680007765647716, -2.599342558260952174 ) ) ;
#14479 = AXIS2_PLACEMENT_3D ( 'NONE', #13375, #13284, #1804 ) ;
#14480 = DIRECTION ( 'NONE',  ( 0.000000000000000000, 0.4999999999999990008, -0.8660254037844391517 ) ) ;
#14481 = CIRCLE ( 'NONE', #2655, 8.000000000000003553 ) ;
#14482 = ORIENTED_EDGE ( 'NONE', *, *, #17682, .T. ) ;
#14483 = AXIS2_PLACEMENT_3D ( 'NONE', #8523, #12614, #5663 ) ;
#14484 = CARTESIAN_POINT ( 'NONE',  ( 2.211161402132902243, 29.62180007765648071, 2.942372952327172442 ) ) ;
#14485 = FACE_OUTER_BOUND ( 'NONE', #4820, .T. ) ;
#14486 = CARTESIAN_POINT ( 'NONE',  ( 3.999999999999996891, -2.343145750507611424, 25.02027108472329786 ) ) ;
#14487 = CARTESIAN_POINT ( 'NONE',  ( 3.999999999999996447, -26.79756825278262511, -9.963095711247856201 ) ) ;
#14488 = ORIENTED_EDGE ( 'NONE', *, *, #11743, .T. ) ;
#14489 = CARTESIAN_POINT ( 'NONE',  ( 3.500000000000000444, 18.25319992234354771, 0.05647727720529520379 ) ) ;
#14490 = CARTESIAN_POINT ( 'NONE',  ( -4.648177544792955347E-16, -29.58051838113927090, -10.99009111451728415 ) ) ;
#14491 = CARTESIAN_POINT ( 'NONE',  ( -5.330712181944245322E-15, -25.49437859686066332, -3.585285685531713451 ) ) ;
#14492 = CARTESIAN_POINT ( 'NONE',  ( 2.798362969681366330, 36.49680007765648071, -2.102939460078824929 ) ) ;
#14493 = ADVANCED_FACE ( 'NONE', ( #13646 ), #10683, .T. ) ;
#14494 = CARTESIAN_POINT ( 'NONE',  ( -2.115076519116425580, 37.37819992234352640, -3.012182706137062738 ) ) ;
#14495 = CARTESIAN_POINT ( 'NONE',  ( -4.243569643750004339, -28.98301395881438580, -12.83906343559744201 ) ) ;
#14496 = CARTESIAN_POINT ( 'NONE',  ( -31.74999999999995737, 0.000000000000000000, 0.000000000000000000 ) ) ;
#14497 = CIRCLE ( 'NONE', #18058, 0.9999999999999991118 ) ;
#14498 = CARTESIAN_POINT ( 'NONE',  ( -2.121784821874996396, -19.12610310501574418, -9.440661126213528931 ) ) ;
#14500 = ADVANCED_FACE ( 'NONE', ( #15146 ), #4391, .T. ) ;
#14499 = VECTOR ( 'NONE', #9440, 1000.000000000000000 ) ;
#14501 = CARTESIAN_POINT ( 'NONE',  ( 8.000000000000001776, 43.00000000000000000, -2.500000000000002220 ) ) ;
#14502 = CARTESIAN_POINT ( 'NONE',  ( -3.706921591972381904E-14, -18.76849698692083379, -9.496498676479825818 ) ) ;
#14503 = DIRECTION ( 'NONE',  ( 0.000000000000000000, 0.000000000000000000, 1.000000000000000000 ) ) ;
#14504 = DIRECTION ( 'NONE',  ( -0.000000000000000000, 1.478898702612462246E-15, 1.000000000000000000 ) ) ;
#14505 = EDGE_LOOP ( 'NONE', ( #5058, #16433, #6496, #9379 ) ) ;
#14506 = VERTEX_POINT ( 'NONE', #9380 ) ;
#14507 = CARTESIAN_POINT ( 'NONE',  ( -6.938893903907228378E-15, 6.938893903907228378E-15, 30.00000000000000000 ) ) ;
#14508 = CARTESIAN_POINT ( 'NONE',  ( 4.000000000000003553, -18.64771640554539545, -6.376536854529449627 ) ) ;
#14509 = ORIENTED_EDGE ( 'NONE', *, *, #5024, .F. ) ;
#14510 = CARTESIAN_POINT ( 'NONE',  ( 1.593127413382953383, 17.87819992234354416, -2.091722143975172532 ) ) ;
#14511 = CARTESIAN_POINT ( 'NONE',  ( -4.243569643750000786, -26.70720613544014199, -13.86036314055876772 ) ) ;
#14512 = LINE ( 'NONE', #9946, #10712 ) ;
#14513 = CARTESIAN_POINT ( 'NONE',  ( 4.299564228933482956E-15, -22.89824732864832768, -15.39439339536058959 ) ) ;
#14514 = CARTESIAN_POINT ( 'NONE',  ( 6.079313232897375130, -14.44302855110184680, -4.023496914807076941 ) ) ;
#14515 = EDGE_LOOP ( 'NONE', ( #2122, #3627, #17829, #13612 ) ) ;
#14516 = CARTESIAN_POINT ( 'NONE',  ( -3.500000000000000444, 40.49680007765648071, 0.05647727720536892260 ) ) ;
#14517 = CARTESIAN_POINT ( 'NONE',  ( -4.243569643750005227, -28.46679516609844995, -12.10182659573734476 ) ) ;
#14518 = VECTOR ( 'NONE', #5708, 999.9999999999998863 ) ;
#14519 = FILL_AREA_STYLE_COLOUR ( '', #7512 ) ;
#14520 = CARTESIAN_POINT ( 'NONE',  ( -2.121784821875005722, -28.38405672417600911, -9.847918799004165891 ) ) ;
#14521 =( BOUNDED_CURVE ( )  B_SPLINE_CURVE ( 2, ( #5272, #2327, #16418, #13614, #6662, #6570, #4056, #9348, #9708 ),
 .UNSPECIFIED., .F., .T. ) 
 B_SPLINE_CURVE_WITH_KNOTS ( ( 3, 2, 2, 2, 3 ),
 ( 0.7327586206896552490, 0.7356321839080459668, 0.7413793103448276245, 0.7471264367816091712, 0.7500000000000000000 ),
 .UNSPECIFIED. ) 
 CURVE ( )  GEOMETRIC_REPRESENTATION_ITEM ( )  RATIONAL_B_SPLINE_CURVE ( ( 0.9330127018922194093, 0.9330127018922206306, 1.000000000000000000, 0.8660254037844387076, 1.000000000000000000, 0.8660254037844387076, 1.000000000000000000, 0.9330127018922194093, 0.9330127018922194093 ) ) 
 REPRESENTATION_ITEM ( '' )  );
#14522 = LINE ( 'NONE', #10136, #1391 ) ;
#14523 = FACE_OUTER_BOUND ( 'NONE', #6536, .T. ) ;
#14524 = CARTESIAN_POINT ( 'NONE',  ( 1.533898589781675205E-14, -28.22544404955499786, -9.054844408877768203 ) ) ;
#14525 = CARTESIAN_POINT ( 'NONE',  ( 4.243569643750003451, -23.25915147027346563, -13.20752085500445894 ) ) ;
#14526 = EDGE_CURVE ( 'NONE', #15102, #12786, #10614, .T. ) ;
#14527 = CARTESIAN_POINT ( 'NONE',  ( 0.000000000000000000, -15.45745613286697839, -10.86990606519494129 ) ) ;
#14528 = CARTESIAN_POINT ( 'NONE',  ( 2.000000000000004441, -17.68033198262726913, -7.008127672724814516 ) ) ;
#14529 = CARTESIAN_POINT ( 'NONE',  ( -0.05938372350926768989, 23.62180007765648071, -2.628655560595669183 ) ) ;
#14530 = ORIENTED_EDGE ( 'NONE', *, *, #5783, .F. ) ;
#14531 = CARTESIAN_POINT ( 'NONE',  ( -2.798362969681365886, 22.74680007765648071, 2.102939460078824929 ) ) ;
#14532 = EDGE_CURVE ( 'NONE', #12253, #14997, #12343, .T. ) ;
#14533 = CARTESIAN_POINT ( 'NONE',  ( -10.00000000000000000, 27.59999999999999432, 2.499999999999998224 ) ) ;
#14534 = DIRECTION ( 'NONE',  ( 0.000000000000000000, 0.000000000000000000, 1.000000000000000000 ) ) ;
#14535 = CARTESIAN_POINT ( 'NONE',  ( 4.000000000000000888, -26.75560164760974047, -13.92947909479903146 ) ) ;
#14536 = DIRECTION ( 'NONE',  ( 0.000000000000000000, 0.9936001553129349961, 0.1129545544106631688 ) ) ;
#14537 = CARTESIAN_POINT ( 'NONE',  ( -2.211161402132839182, 21.62819992234354771, 2.942372952327218627 ) ) ;
#14538 = VERTEX_POINT ( 'NONE', #2631 ) ;
#14539 = CARTESIAN_POINT ( 'NONE',  ( -2.121784821874996396, -20.93286887952152497, -12.02099006572386486 ) ) ;
#14540 = CARTESIAN_POINT ( 'NONE',  ( -3.500000000000000444, 17.99680007765647716, 0.05647727720536892260 ) ) ;
#14541 = ORIENTED_EDGE ( 'NONE', *, *, #17696, .T. ) ;
#14542 = CARTESIAN_POINT ( 'NONE',  ( 3.999999999999996447, -21.95801707177565731, -3.051500338566227377 ) ) ;
#14543 = CARTESIAN_POINT ( 'NONE',  ( 2.121784821874994176, -28.88952095871037429, -10.56979653803383989 ) ) ;
#14544 = CARTESIAN_POINT ( 'NONE',  ( -4.000000000000000888, -25.33599996764090534, -11.90207778518377246 ) ) ;
#14545 = CIRCLE ( 'NONE', #8586, 10.00000000000000000 ) ;
#14546 = CARTESIAN_POINT ( 'NONE',  ( -1.734723475976807094E-15, 34.19999999999999574, -10.50000000000000178 ) ) ;
#14547 = CARTESIAN_POINT ( 'NONE',  ( 0.000000000000000000, 3.518949890710770134, -4.119968255444916849E-15 ) ) ;
#14548 = CARTESIAN_POINT ( 'NONE',  ( 2.121784821875004390, -18.91101194138411046, -9.133479109605152857 ) ) ;
#14549 = ADVANCED_FACE ( 'NONE', ( #18220 ), #8270, .T. ) ;
#14550 = ORIENTED_EDGE ( 'NONE', *, *, #14316, .F. ) ;
#14551 = FACE_OUTER_BOUND ( 'NONE', #631, .T. ) ;
#14552 = ADVANCED_FACE ( 'NONE', ( #14973 ), #16449, .T. ) ;
#14553 = DIRECTION ( 'NONE',  ( 0.000000000000000000, 1.000000000000000000, 0.000000000000000000 ) ) ;
#14554 = CARTESIAN_POINT ( 'NONE',  ( 4.898587196589409870E-16, 4.000000000000007105, -4.000000000000000000 ) ) ;
#14555 = ADVANCED_FACE ( 'NONE', ( #18035 ), #11090, .T. ) ;
#14556 = ORIENTED_EDGE ( 'NONE', *, *, #5910, .F. ) ;
#14557 = VERTEX_POINT ( 'NONE', #15027 ) ;
#14558 = CYLINDRICAL_SURFACE ( 'NONE', #8358, 4.000000000000000000 ) ;
#14559 = CARTESIAN_POINT ( 'NONE',  ( 0.000000000000000000, 0.000000000000000000, 0.000000000000000000 ) ) ;
#14560 = CARTESIAN_POINT ( 'NONE',  ( 1.336863392178569754, 26.25319992234354416, 4.297206761780648421 ) ) ;
#14561 = CARTESIAN_POINT ( 'NONE',  ( -3.481649420246394566, 27.12819992234354771, -1.193696214020467883 ) ) ;
#14562 = CARTESIAN_POINT ( 'NONE',  ( 1.497042530366522461, 23.62819992234354416, 2.161531897785029965 ) ) ;
#14563 = ORIENTED_EDGE ( 'NONE', *, *, #3037, .F. ) ;
#14564 = MECHANICAL_DESIGN_GEOMETRIC_PRESENTATION_REPRESENTATION (  '', ( #7725 ), #3591 ) ;
#14565 = CARTESIAN_POINT ( 'NONE',  ( 1.336863392178569754, 38.75319992234354061, 4.297206761780648421 ) ) ;
#14566 = CARTESIAN_POINT ( 'NONE',  ( -3.999999999999997335, -20.04580896844610649, -8.373219961477115447 ) ) ;
#14567 = EDGE_LOOP ( 'NONE', ( #14814, #10128, #11340, #9053 ) ) ;
#14568 = FACE_OUTER_BOUND ( 'NONE', #9362, .T. ) ;
#14569 = CARTESIAN_POINT ( 'NONE',  ( 2.115076519116362963, 28.87180007765647716, -3.012182706137107147 ) ) ;
#14570 = CARTESIAN_POINT ( 'NONE',  ( -7.076011672040958267, -12.11284110773042144, 11.47761944861337469 ) ) ;
#14571 = CARTESIAN_POINT ( 'NONE',  ( -2.121784821875005722, -24.77052517516444752, -4.687260919983497587 ) ) ;
#14572 = CARTESIAN_POINT ( 'NONE',  ( -2.829195390882805139, 30.87180007765647716, -3.793023760679206102 ) ) ;
#14573 = DIRECTION ( 'NONE',  ( -0.000000000000000000, -1.000000000000000000, -0.000000000000000000 ) ) ;
#14574 = ORIENTED_EDGE ( 'NONE', *, *, #15615, .T. ) ;
#14575 = CARTESIAN_POINT ( 'NONE',  ( -1.135272562821090014, 33.49680007765648071, -3.311245368580554072 ) ) ;
#14576 = CARTESIAN_POINT ( 'NONE',  ( 14.20000000000000107, 0.000000000000000000, 0.000000000000000000 ) ) ;
#14577 = CYLINDRICAL_SURFACE ( 'NONE', #5114, 2.149999999999995470 ) ;
#14578 = DIRECTION ( 'NONE',  ( -3.373073425510457965E-16, 0.000000000000000000, -1.000000000000000000 ) ) ;
#14579 = CARTESIAN_POINT ( 'NONE',  ( 4.000000000000000888, -24.88430852330952447, -11.25699554929942003 ) ) ;
#14580 = ORIENTED_EDGE ( 'NONE', *, *, #3989, .T. ) ;
#14581 = CARTESIAN_POINT ( 'NONE',  ( -2.798362969681409851, 27.25319992234354771, -2.102939460078765421 ) ) ;
#14582 = CARTESIAN_POINT ( 'NONE',  ( -9.000000000000001776, 29.79999999999999716, 2.499999999999998224 ) ) ;
#14583 = CARTESIAN_POINT ( 'NONE',  ( 2.121784821874994176, -24.46939754608015605, -4.257206096731771083 ) ) ;
#14584 = CARTESIAN_POINT ( 'NONE',  ( -2.500000000000001332, 20.49680007765648071, 0.05647727720535858364 ) ) ;
#14585 = VECTOR ( 'NONE', #1122, 1000.000000000000000 ) ;
#14586 = EDGE_CURVE ( 'NONE', #7792, #4253, #12224, .T. ) ;
#14587 = CARTESIAN_POINT ( 'NONE',  ( 2.864755990943222308, 35.50319992234354771, -2.011557305968548093 ) ) ;
#14588 = CARTESIAN_POINT ( 'NONE',  ( 4.243569643750003451, -25.09818091932399398, -15.83392709700605039 ) ) ;
#14589 = CARTESIAN_POINT ( 'NONE',  ( -4.000000000000004441, -28.69037049274105300, -12.66629745740154434 ) ) ;
#14590 = PRESENTATION_LAYER_ASSIGNMENT (  '', '', ( #12197 ) ) ;
#14591 = CARTESIAN_POINT ( 'NONE',  ( 4.730628863548789710E-15, -16.59548390881375468, -7.962307421154977582 ) ) ;
#14592 = CARTESIAN_POINT ( 'NONE',  ( -1.734723475976807094E-15, 23.19999999999999574, -12.50000000000000000 ) ) ;
#14593 = CARTESIAN_POINT ( 'NONE',  ( 0.2979626678773949489, -10.00000000000000178, -4.943697222988730822 ) ) ;
#14594 = AXIS2_PLACEMENT_3D ( 'NONE', #11444, #15731, #3123 ) ;
#14595 = DIRECTION ( 'NONE',  ( 0.000000000000000000, 0.000000000000000000, 1.000000000000000000 ) ) ;
#14596 = AXIS2_PLACEMENT_3D ( 'NONE', #14559, #11848, #11660 ) ;
#14597 = DIRECTION ( 'NONE',  ( 0.000000000000000000, 0.000000000000000000, -1.000000000000000000 ) ) ;
#14598 = ORIENTED_EDGE ( 'NONE', *, *, #8583, .F. ) ;
#14599 = ORIENTED_EDGE ( 'NONE', *, *, #6934, .F. ) ;
#14600 = SURFACE_STYLE_FILL_AREA ( #16172 ) ;
#14601 = EDGE_CURVE ( 'NONE', #4985, #13486, #15964, .T. ) ;
#14602 = DIRECTION ( 'NONE',  ( 1.000000000000000000, 0.000000000000000000, -4.336808689942021680E-16 ) ) ;
#14603 = AXIS2_PLACEMENT_3D ( 'NONE', #9802, #8672, #5812 ) ;
#14604 = ORIENTED_EDGE ( 'NONE', *, *, #5247, .F. ) ;
#14605 = CARTESIAN_POINT ( 'NONE',  ( 1.593127413382953383, 27.87819992234355126, -2.091722143975172532 ) ) ;
#14606 = CARTESIAN_POINT ( 'NONE',  ( -4.243569643750005227, -28.17642209519573271, -11.68713087331604150 ) ) ;
#14607 = CARTESIAN_POINT ( 'NONE',  ( -3.481649420246369697, 17.87180007765648071, 1.193696214020542490 ) ) ;
#14608 = EDGE_CURVE ( 'NONE', #5643, #3185, #17760, .T. ) ;
#14609 = CARTESIAN_POINT ( 'NONE',  ( 13.80999999999999872, 0.000000000000000000, 0.000000000000000000 ) ) ;
#14610 = LINE ( 'NONE', #6154, #17684 ) ;
#14611 = EDGE_LOOP ( 'NONE', ( #1621, #13132 ) ) ;
#14612 = TOROIDAL_SURFACE ( 'NONE', #11033, 9.000000000000003553, 0.9999999999999991118 ) ;
#14613 = CARTESIAN_POINT ( 'NONE',  ( 2.798362969681366330, 38.99680007765647360, -2.102939460078824929 ) ) ;
#14614 = CIRCLE ( 'NONE', #993, 0.9999999999999991118 ) ;
#14615 = CARTESIAN_POINT ( 'NONE',  ( 2.610817815249942608, -22.30731692868453564, -2.152029956302548008 ) ) ;
#14616 = CARTESIAN_POINT ( 'NONE',  ( -3.500000000000000444, 39.50319992234354771, -0.05647727720529563400 ) ) ;
#14617 = CARTESIAN_POINT ( 'NONE',  ( -4.243569643749998122, -22.14067741938892908, -11.61017436864092112 ) ) ;
#14618 = DIRECTION ( 'NONE',  ( -0.000000000000000000, -0.5735764363510414965, -0.8191520442889950182 ) ) ;
#14619 = DIRECTION ( 'NONE',  ( -1.000000000000000000, -0.000000000000000000, -0.000000000000000000 ) ) ;
#14620 = DIRECTION ( 'NONE',  ( -0.000000000000000000, -1.000000000000000000, -0.000000000000000000 ) ) ;
#14621 = MANIFOLD_SOLID_BREP ( 'LPattern6[6]', #16230 ) ;
#14622 = CARTESIAN_POINT ( 'NONE',  ( -5.330712181944245322E-15, -26.78492557865051538, -5.428377785181952575 ) ) ;
#14623 = DIRECTION ( 'NONE',  ( 0.000000000000000000, -1.000000000000000000, 0.000000000000000000 ) ) ;
#14624 = AXIS2_PLACEMENT_3D ( 'NONE', #5533, #9795, #17137 ) ;
#14625 = DIRECTION ( 'NONE',  ( -0.000000000000000000, -0.5735764363510414965, -0.8191520442889950182 ) ) ;
#14626 = CARTESIAN_POINT ( 'NONE',  ( 2.481649420246374138, 21.62180007765648426, -0.8687765177876252132 ) ) ;
#14627 = EDGE_CURVE ( 'NONE', #4281, #16392, #11687, .T. ) ;
#14628 = CARTESIAN_POINT ( 'NONE',  ( 0.000000000000000000, 5.977523610840987267, 32.81826849749789687 ) ) ;
#14629 = CARTESIAN_POINT ( 'NONE',  ( 1.135272562821090458, 24.74680007765647716, 3.311245368580554072 ) ) ;
#14630 = CARTESIAN_POINT ( 'NONE',  ( 1.533898589781675205E-14, -27.77375260663349366, -8.409762175006950002 ) ) ;
#14631 = CARTESIAN_POINT ( 'NONE',  ( -3.999999999999997335, -24.49819605632600883, -14.73188770627720245 ) ) ;
#14632 = LINE ( 'NONE', #14917, #16397 ) ;
#14633 = CARTESIAN_POINT ( 'NONE',  ( -3.481649420246394122, 17.12819992234354061, -1.193696214020467883 ) ) ;
#14634 = VERTEX_POINT ( 'NONE', #9533 ) ;
#14635 = CARTESIAN_POINT ( 'NONE',  ( -4.243569643750004339, -25.11137301344485451, -7.309787136646725081 ) ) ;
#14636 = CARTESIAN_POINT ( 'NONE',  ( -2.798362969681365886, 20.24680007765647716, 2.102939460078824929 ) ) ;
#14637 =( BOUNDED_CURVE ( )  B_SPLINE_CURVE ( 2, ( #9031, #2007, #1723, #7545, #4673, #11622, #16004, #4581, #10227 ),
 .UNSPECIFIED., .F., .T. ) 
 B_SPLINE_CURVE_WITH_KNOTS ( ( 3, 2, 2, 2, 3 ),
 ( 0.2500000000000000000, 0.2528735632183908288, 0.2586206896551724310, 0.2643678160919540332, 0.2672413793103448620 ),
 .UNSPECIFIED. ) 
 CURVE ( )  GEOMETRIC_REPRESENTATION_ITEM ( )  RATIONAL_B_SPLINE_CURVE ( ( 0.9330127018922194093, 0.9330127018922190762, 1.000000000000000000, 0.8660254037844387076, 1.000000000000000000, 0.8660254037844387076, 1.000000000000000000, 0.9330127018922187432, 0.9330127018922194093 ) ) 
 REPRESENTATION_ITEM ( '' )  );
#14638 = ORIENTED_EDGE ( 'NONE', *, *, #4950, .T. ) ;
#14639 = AXIS2_PLACEMENT_3D ( 'NONE', #8281, #6522, #17862 ) ;
#14640 = CARTESIAN_POINT ( 'NONE',  ( -1.734723475976807094E-15, 38.59999999999999432, -2.500000000000000000 ) ) ;
#14641 = DIRECTION ( 'NONE',  ( -0.000000000000000000, -1.000000000000000000, -0.000000000000000000 ) ) ;
#14642 = CARTESIAN_POINT ( 'NONE',  ( -2.121784821874996396, -22.48152525766933962, -14.23270058530414950 ) ) ;
#14643 = CARTESIAN_POINT ( 'NONE',  ( 4.000000000000003553, -24.77781456834220464, -15.13122432686131802 ) ) ;
#14644 = CARTESIAN_POINT ( 'NONE',  ( -4.000000000000000888, -25.85221876035684474, -12.63931462504386793 ) ) ;
#14645 = CARTESIAN_POINT ( 'NONE',  ( -2.000000000000005773, -27.80797090842707320, -9.392941296374171856 ) ) ;
#14646 = CARTESIAN_POINT ( 'NONE',  ( -4.243569643749997233, -17.78508135584820948, -5.389738532321366904 ) ) ;
#14647 = ORIENTED_EDGE ( 'NONE', *, *, #11683, .T. ) ;
#14648 = CARTESIAN_POINT ( 'NONE',  ( 0.000000000000000000, -27.20729309053124112, -14.57456132866985321 ) ) ;
#14649 = CARTESIAN_POINT ( 'NONE',  ( 3.999999999999996447, -25.05532982807127951, -7.474921377726800209 ) ) ;
#14650 = TOROIDAL_SURFACE ( 'NONE', #5748, 9.000000000000001776, 0.9999999999999991118 ) ;
#14651 = DIRECTION ( 'NONE',  ( 0.000000000000000000, 0.000000000000000000, -1.000000000000000000 ) ) ;
#14652 = VERTEX_POINT ( 'NONE', #4155 ) ;
#14653 = ORIENTED_EDGE ( 'NONE', *, *, #6107, .T. ) ;
#14654 = DIRECTION ( 'NONE',  ( 1.000000000000000000, 0.000000000000000000, 0.000000000000000000 ) ) ;
#14655 = DIRECTION ( 'NONE',  ( 0.000000000000000000, 0.000000000000000000, 1.000000000000000000 ) ) ;
#14656 = CARTESIAN_POINT ( 'NONE',  ( -3.673772985318163098, 29.25319992234354416, 2.599342558261029001 ) ) ;
#14657 = CARTESIAN_POINT ( 'NONE',  ( -2.211161402132838738, 36.62819992234354061, 2.942372952327218183 ) ) ;
#14658 = CARTESIAN_POINT ( 'NONE',  ( 0.05938372350921204690, 17.62819992234354416, -2.628655560595669183 ) ) ;
#14659 = MANIFOLD_SOLID_BREP ( 'LPattern6[11]', #14444 ) ;
#14660 = VERTEX_POINT ( 'NONE', #8490 ) ;
#14661 = CARTESIAN_POINT ( 'NONE',  ( 0.05938372350929014415, 17.37180007765647716, 4.731580009072201776 ) ) ;
#14662 = CARTESIAN_POINT ( 'NONE',  ( 4.000000000000003553, -20.90617362297267690, -9.601948027910603756 ) ) ;
#14663 = ORIENTED_EDGE ( 'NONE', *, *, #9829, .F. ) ;
#14664 = EDGE_CURVE ( 'NONE', #13443, #4345, #15212, .T. ) ;
#14665 = CARTESIAN_POINT ( 'NONE',  ( -1.661723472263481630E-14, -21.34959095050052014, -13.18268287578030318 ) ) ;
#14666 = EDGE_CURVE ( 'NONE', #6640, #3912, #9803, .T. ) ;
#14667 = CARTESIAN_POINT ( 'NONE',  ( 1.135272562821090458, 27.24680007765648071, 3.311245368580554072 ) ) ;
#14668 = CARTESIAN_POINT ( 'NONE',  ( -8.000000000000003553, 25.39999999999999503, -2.500000000000001776 ) ) ;
#14669 = ADVANCED_FACE ( 'NONE', ( #14067 ), #5004, .T. ) ;
#14670 = CARTESIAN_POINT ( 'NONE',  ( 2.121784821874994176, -24.98561633879609545, -4.994442936591867443 ) ) ;
#14671 = CARTESIAN_POINT ( 'NONE',  ( -1.444289557196047014, 33.49680007765648071, -4.262301884875704161 ) ) ;
#14672 = EDGE_CURVE ( 'NONE', #8639, #1548, #14165, .T. ) ;
#14673 = CARTESIAN_POINT ( 'NONE',  ( 4.000000000000000000, -3.518949890710769246, 4.119968255444916849E-15 ) ) ;
#14674 = ORIENTED_EDGE ( 'NONE', *, *, #15884, .T. ) ;
#14675 = CARTESIAN_POINT ( 'NONE',  ( -2.864755990943265829, 30.74680007765647716, -2.011557305968488141 ) ) ;
#14676 = CARTESIAN_POINT ( 'NONE',  ( 13.00000000000000178, 15.00000000000000178, -25.00000000000000355 ) ) ;
#14677 = DIRECTION ( 'NONE',  ( 0.000000000000000000, 0.000000000000000000, -1.000000000000000000 ) ) ;
#14678 = DIRECTION ( 'NONE',  ( 0.000000000000000000, 1.000000000000000000, 0.000000000000000000 ) ) ;
#14679 = CARTESIAN_POINT ( 'NONE',  ( -10.00000000000000178, 16.59999999999999787, -2.500000000000001776 ) ) ;
#14680 = ORIENTED_EDGE ( 'NONE', *, *, #6701, .F. ) ;
#14681 = CARTESIAN_POINT ( 'NONE',  ( -2.211161402132839182, 29.12819992234354771, 2.942372952327218627 ) ) ;
#14682 = DIRECTION ( 'NONE',  ( 0.000000000000000000, 0.000000000000000000, -1.000000000000000000 ) ) ;
#14683 = CARTESIAN_POINT ( 'NONE',  ( -4.243569643750005227, -23.27234356439432972, -4.683380894645135406 ) ) ;
#14684 = CARTESIAN_POINT ( 'NONE',  ( 2.481649420246374138, 21.62180007765648426, -0.8687765177876252132 ) ) ;
#14685 = ADVANCED_FACE ( 'NONE', ( #12493 ), #18187, .F. ) ;
#14686 = CARTESIAN_POINT ( 'NONE',  ( 0.05938372350919016857, 20.12819992234354416, -4.731580009072201776 ) ) ;
#14687 = CARTESIAN_POINT ( 'NONE',  ( -4.243569643750004339, -28.72490456245641255, -12.47044501566739427 ) ) ;
#14688 = CARTESIAN_POINT ( 'NONE',  ( -4.000000000000000888, -25.78769141056240954, -12.54716001905459066 ) ) ;
#14689 = CARTESIAN_POINT ( 'NONE',  ( -4.243569643750000786, -21.31917248646755070, -6.165453624519022569 ) ) ;
#14690 = DIRECTION ( 'NONE',  ( -3.469446951953613696E-16, -0.000000000000000000, -1.000000000000000000 ) ) ;
#14691 = LINE ( 'NONE', #16444, #17099 ) ;
#14692 = CARTESIAN_POINT ( 'NONE',  ( 1.533898589781675205E-14, -27.70922525683905846, -8.317607569017670954 ) ) ;
#14693 = CYLINDRICAL_SURFACE ( 'NONE', #12677, 7.000000000000000000 ) ;
#14694 = ORIENTED_EDGE ( 'NONE', *, *, #17675, .F. ) ;
#14695 = ORIENTED_EDGE ( 'NONE', *, *, #7940, .F. ) ;
#14696 = PRESENTATION_STYLE_ASSIGNMENT (( #692 ) ) ;
#14697 = DIRECTION ( 'NONE',  ( -1.000000000000000000, 0.000000000000000000, 0.000000000000000000 ) ) ;
#14698 = CARTESIAN_POINT ( 'NONE',  ( 1.071796769724485232, -23.89058496054513370, -2.864024041400317078 ) ) ;
#14699 = ORIENTED_EDGE ( 'NONE', *, *, #7625, .T. ) ;
#14700 = CARTESIAN_POINT ( 'NONE',  ( -0.8262555684460826111, 26.50319992234354771, 2.360188852285421302 ) ) ;
#14701 = DIRECTION ( 'NONE',  ( 1.000000000000000000, 0.000000000000000000, 0.000000000000000000 ) ) ;
#14702 = CARTESIAN_POINT ( 'NONE',  ( 4.243569643750000786, -25.02949505911335137, -11.46434341101345389 ) ) ;
#14703 = CARTESIAN_POINT ( 'NONE',  ( 2.115076519116362963, 23.87180007765647005, -3.012182706137107147 ) ) ;
#14704 = CIRCLE ( 'NONE', #3738, 0.9999999999999991118 ) ;
#14705 = PLANE ( 'NONE',  #18200 ) ;
#14706 = AXIS2_PLACEMENT_3D ( 'NONE', #18004, #5274, #6844 ) ;
#14707 = CARTESIAN_POINT ( 'NONE',  ( -2.797762022055394482E-14, -10.00000000000000178, -12.59063537424807677 ) ) ;
#14708 = CARTESIAN_POINT ( 'NONE',  ( 2.121784821875004390, -22.52454349039567205, -14.29413698862582294 ) ) ;
#14709 = CARTESIAN_POINT ( 'NONE',  ( -10.00000000000000000, 36.39999999999999147, 2.499999999999996003 ) ) ;
#14710 = CARTESIAN_POINT ( 'NONE',  ( 4.730628863548789710E-15, -19.66053299056463288, -12.33965115782429400 ) ) ;
#14711 = DIRECTION ( 'NONE',  ( -0.000000000000000000, -0.5735764363510414965, -0.8191520442889950182 ) ) ;
#14712 = CARTESIAN_POINT ( 'NONE',  ( 0.000000000000000000, 5.000000000000000000, 0.000000000000000000 ) ) ;
#14713 = CARTESIAN_POINT ( 'NONE',  ( -9.000000000000003553, 36.39999999999999147, -2.500000000000001776 ) ) ;
#14714 = VECTOR ( 'NONE', #1819, 1000.000000000000000 ) ;
#14715 = CARTESIAN_POINT ( 'NONE',  ( -2.121784821874996396, -20.90060520497677743, -11.97491276323260756 ) ) ;
#14716 = CARTESIAN_POINT ( 'NONE',  ( -1.734723475976807094E-15, 34.19999999999999574, -2.500000000000000000 ) ) ;
#14717 = CARTESIAN_POINT ( 'NONE',  ( -4.000000000000004441, -21.52783474451236145, -2.437136305349486332 ) ) ;
#14718 = CARTESIAN_POINT ( 'NONE',  ( 0.7188294034286049072, 33.74680007765648071, -2.395093729190366005 ) ) ;
#14719 = ORIENTED_EDGE ( 'NONE', *, *, #8982, .F. ) ;
#14720 = CARTESIAN_POINT ( 'NONE',  ( -3.500000000000000444, 30.49680007765647716, 0.05647727720536892260 ) ) ;
#14721 = CARTESIAN_POINT ( 'NONE',  ( 1.071796769724485454, -20.58678946214543970, -12.09328945064608085 ) ) ;
#14722 = PRODUCT_CONTEXT ( 'NONE', #264, 'mechanical' ) ;
#14723 = CARTESIAN_POINT ( 'NONE',  ( 4.713407268011036227E-15, -21.61702609051053514, -14.64346846959108284 ) ) ;
#14724 = CARTESIAN_POINT ( 'NONE',  ( 0.000000000000000000, 34.19999999999999574, 2.500000000000000000 ) ) ;
#14725 = CARTESIAN_POINT ( 'NONE',  ( -2.115076519116425580, 17.37819992234354771, -3.012182706137062738 ) ) ;
#14726 = ORIENTED_EDGE ( 'NONE', *, *, #16603, .T. ) ;
#14727 = CARTESIAN_POINT ( 'NONE',  ( 4.730628863548789710E-15, -18.66035907967750163, -10.91125478059535858 ) ) ;
#14728 = CARTESIAN_POINT ( 'NONE',  ( 1.444289557196047680, 39.74680007765648071, 4.262301884875704161 ) ) ;
#14729 = AXIS2_PLACEMENT_3D ( 'NONE', #6704, #5683, #14120 ) ;
#14730 = EDGE_LOOP ( 'NONE', ( #3691, #6636, #6191, #3960 ) ) ;
#14731 = FILL_AREA_STYLE_COLOUR ( '', #16091 ) ;
#14732 = EDGE_CURVE ( 'NONE', #8704, #13968, #11195, .T. ) ;
#14733 = DIRECTION ( 'NONE',  ( 1.000000000000000000, 0.000000000000000000, 0.000000000000000000 ) ) ;
#14734 = CARTESIAN_POINT ( 'NONE',  ( -2.121784821875005722, -28.15821100236278696, -9.525377681565375454 ) ) ;
#14735 = DIRECTION ( 'NONE',  ( -0.000000000000000000, -1.000000000000000000, -0.000000000000000000 ) ) ;
#14736 = CARTESIAN_POINT ( 'NONE',  ( 9.320906609362770823, -9.992678237866394753, -2.177225805445022644 ) ) ;
#14737 = LINE ( 'NONE', #13328, #2883 ) ;
#14738 = CARTESIAN_POINT ( 'NONE',  ( 4.243569643750000786, -19.89957080649872623, -4.138052314903757356 ) ) ;
#14739 = EDGE_LOOP ( 'NONE', ( #8269, #4153, #9245, #1583 ) ) ;
#14740 = CARTESIAN_POINT ( 'NONE',  ( -1.661723472263481630E-14, -20.76884480799014554, -12.35329142993093576 ) ) ;
#14741 = CARTESIAN_POINT ( 'NONE',  ( 3.999999999999996447, -24.79722043171331336, -7.106302957796752473 ) ) ;
#14742 = LINE ( 'NONE', #13334, #11174 ) ;
#14743 = ORIENTED_EDGE ( 'NONE', *, *, #16967, .T. ) ;
#14744 = VECTOR ( 'NONE', #6776, 1000.000000000000000 ) ;
#14745 = ORIENTED_EDGE ( 'NONE', *, *, #8865, .T. ) ;
#14746 = CARTESIAN_POINT ( 'NONE',  ( 1.999999999999994449, -27.05515183642128108, -8.317804239251627152 ) ) ;
#14747 = CARTESIAN_POINT ( 'NONE',  ( -8.999999999999992895, -13.00000000000000000, -3.713574246709377746 ) ) ;
#14748 = SHAPE_DEFINITION_REPRESENTATION ( #3532, #15868 ) ;
#14749 = CARTESIAN_POINT ( 'NONE',  ( 2.733110507866328920, 23.62819992234354416, 3.862833514489095510 ) ) ;
#14750 = CARTESIAN_POINT ( 'NONE',  ( -3.481649420246394566, 32.12819992234354061, -1.193696214020467883 ) ) ;
#14751 = CARTESIAN_POINT ( 'NONE',  ( -0.8262555684460826111, 21.50319992234354771, 2.360188852285421302 ) ) ;
#14752 = EDGE_LOOP ( 'NONE', ( #12151, #9398, #5107, #15751 ) ) ;
#14753 = CARTESIAN_POINT ( 'NONE',  ( 3.607379964056306676, 21.49680007765647360, -2.690724712371305838 ) ) ;
#14754 = CARTESIAN_POINT ( 'NONE',  ( 4.000000000000000888, -21.78699576701389873, -6.833574510138848090 ) ) ;
#14755 = ORIENTED_EDGE ( 'NONE', *, *, #4312, .F. ) ;
#14756 = CIRCLE ( 'NONE', #7909, 0.9999999999999991118 ) ;
#14757 = DIRECTION ( 'NONE',  ( -0.000000000000000000, 1.000000000000000000, -0.000000000000000000 ) ) ;
#14758 = AXIS2_PLACEMENT_3D ( 'NONE', #7267, #1924, #4498 ) ;
#14759 = CARTESIAN_POINT ( 'NONE',  ( 2.798362969681366330, 38.99680007765647360, -2.102939460078824929 ) ) ;
#14760 = DIRECTION ( 'NONE',  ( -0.000000000000000000, -1.000000000000000000, -0.000000000000000000 ) ) ;
#14761 = CARTESIAN_POINT ( 'NONE',  ( -4.243569643750004339, -23.53045296075229942, -5.051999314575183142 ) ) ;
#14762 = CARTESIAN_POINT ( 'NONE',  ( 4.243569643749996345, -25.54155534070815392, -7.924151169863466571 ) ) ;
#14763 = DIRECTION ( 'NONE',  ( 0.000000000000000000, 0.000000000000000000, 1.000000000000000000 ) ) ;
#14764 = ORIENTED_EDGE ( 'NONE', *, *, #11571, .T. ) ;
#14765 = CARTESIAN_POINT ( 'NONE',  ( -4.950315044628286643, -10.00000000000096811, 20.01801554166341646 ) ) ;
#14766 = EDGE_CURVE ( 'NONE', #1083, #11658, #3243, .T. ) ;
#14767 = DIRECTION ( 'NONE',  ( 0.000000000000000000, 0.000000000000000000, -1.000000000000000000 ) ) ;
#14768 = CARTESIAN_POINT ( 'NONE',  ( 3.999999999999996447, -24.02289224263940426, -6.000447698006609265 ) ) ;
#14769 = CARTESIAN_POINT ( 'NONE',  ( -4.243569643749997233, -25.01214445387132912, -15.71105429036270351 ) ) ;
#14770 = ORIENTED_EDGE ( 'NONE', *, *, #8744, .F. ) ;
#14771=STYLED_ITEM('',(#18389),#13901);
#14772 = CARTESIAN_POINT ( 'NONE',  ( 2.864755990943222308, 25.50319992234354771, -2.011557305968548093 ) ) ;
#14773 = DIRECTION ( 'NONE',  ( 0.000000000000000000, 0.000000000000000000, -1.000000000000000000 ) ) ;
#14774 = VECTOR ( 'NONE', #9648, 1000.000000000000000 ) ;
#14775 = CARTESIAN_POINT ( 'NONE',  ( 2.121784821875004390, -18.36252947412342351, -8.350164967253801862 ) ) ;
#14776 = CARTESIAN_POINT ( 'NONE',  ( -0.8262555684461330152, 23.49680007765647716, -2.360188852285403982 ) ) ;
#14777 = CARTESIAN_POINT ( 'NONE',  ( 1.336863392178569754, 21.25319992234354771, 4.297206761780648421 ) ) ;
#14778 = CARTESIAN_POINT ( 'NONE',  ( -4.243569643749998122, -24.75403505751336297, -15.34243587043265400 ) ) ;
#14779 = CARTESIAN_POINT ( 'NONE',  ( 4.000000000000003553, -24.77781456834220464, -15.13122432686131802 ) ) ;
#14780 = CARTESIAN_POINT ( 'NONE',  ( 4.243569643750003451, -18.90355540673274248, -6.987085018684902948 ) ) ;
#14781 = CARTESIAN_POINT ( 'NONE',  ( -2.733110507866247652, 37.62180007765646650, 3.862833514489154574 ) ) ;
#14782 = CIRCLE ( 'NONE', #2641, 0.9999999999999991118 ) ;
#14783 = CIRCLE ( 'NONE', #16859, 5.000000000000000000 ) ;
#14784 = DIRECTION ( 'NONE',  ( -0.000000000000000000, -0.000000000000000000, -1.000000000000000000 ) ) ;
#14785 = EDGE_CURVE ( 'NONE', #17369, #7045, #8844, .T. ) ;
#14786 = CARTESIAN_POINT ( 'NONE',  ( 7.347880794884120722E-16, 13.00000000000000178, -6.000000000000000888 ) ) ;
#14787 = CARTESIAN_POINT ( 'NONE',  ( 0.000000000000000000, 13.00000000000000178, -4.000000000000000888 ) ) ;
#14788 = EDGE_LOOP ( 'NONE', ( #3375, #11332, #2703, #18095 ) ) ;
#14789 = VERTEX_POINT ( 'NONE', #256 ) ;
#14790 = CARTESIAN_POINT ( 'NONE',  ( -2.121784821875005722, -22.70565000430070057, -1.738313560543115477 ) ) ;
#14791 = EDGE_CURVE ( 'NONE', #2204, #2269, #17162, .T. ) ;
#14792 = LINE ( 'NONE', #10309, #17504 ) ;
#14793 = ORIENTED_EDGE ( 'NONE', *, *, #12871, .F. ) ;
#14794 = CARTESIAN_POINT ( 'NONE',  ( 1.593127413382953383, 25.37819992234354416, -2.091722143975172532 ) ) ;
#14795 = EDGE_CURVE ( 'NONE', #2069, #9984, #9893, .T. ) ;
#14796 = CARTESIAN_POINT ( 'NONE',  ( -2.121784821875005722, -28.12594732781803941, -9.479300379074118155 ) ) ;
#14797 = CARTESIAN_POINT ( 'NONE',  ( -3.518350579753630747, 23.12180007765647716, -1.080741659609802729 ) ) ;
#14798 = TOROIDAL_SURFACE ( 'NONE', #5299, 9.000000000000003553, 0.9999999999999991118 ) ;
#14799 = DIRECTION ( 'NONE',  ( 0.000000000000000000, 0.000000000000000000, -1.000000000000000000 ) ) ;
#14800 = CARTESIAN_POINT ( 'NONE',  ( 3.537103074283489246, -10.00000000000000178, -11.53856502750720203 ) ) ;
#14801 = CARTESIAN_POINT ( 'NONE',  ( -4.243569643750000786, -24.93270403547910874, -11.32611150353969087 ) ) ;
#14802 = LINE ( 'NONE', #13018, #8133 ) ;
#14803 = CARTESIAN_POINT ( 'NONE',  ( 4.243569643750000786, -24.25516687003944938, -10.35848815122331068 ) ) ;
#14804 = DIRECTION ( 'NONE',  ( 0.000000000000000000, 0.000000000000000000, 1.000000000000000000 ) ) ;
#14805 = CIRCLE ( 'NONE', #4132, 0.9999999999999991118 ) ;
#14806 = DIRECTION ( 'NONE',  ( 0.000000000000000000, 0.000000000000000000, -1.000000000000000000 ) ) ;
#14807 = AXIS2_PLACEMENT_3D ( 'NONE', #1869, #17648, #7499 ) ;
#14808 = DIRECTION ( 'NONE',  ( 0.000000000000000000, 0.000000000000000000, -1.000000000000000000 ) ) ;
#14809 = CARTESIAN_POINT ( 'NONE',  ( 4.730628863548789710E-15, -19.66053299056463288, -12.33965115782429400 ) ) ;
#14810 = ORIENTED_EDGE ( 'NONE', *, *, #10761, .T. ) ;
#14811 = DIRECTION ( 'NONE',  ( -0.000000000000000000, 1.000000000000000000, -0.000000000000000000 ) ) ;
#14812 = DIRECTION ( 'NONE',  ( 0.000000000000000000, 0.8191520442889952403, -0.5735764363510413855 ) ) ;
#14813 = CARTESIAN_POINT ( 'NONE',  ( 2.481649420246374138, 26.62180007765648426, -0.8687765177876252132 ) ) ;
#14814 = ORIENTED_EDGE ( 'NONE', *, *, #11357, .F. ) ;
#14815 = CARTESIAN_POINT ( 'NONE',  ( -1.135272562821090014, 25.99680007765648071, -3.311245368580554072 ) ) ;
#14816 = CARTESIAN_POINT ( 'NONE',  ( -1.071796769724487675, -23.40293942064543486, -16.11516840056477662 ) ) ;
#14817 = APPLICATION_PROTOCOL_DEFINITION ( 'draft international standard', 'automotive_design', 1998, #5108 ) ;
#14818 = CARTESIAN_POINT ( 'NONE',  ( 0.000000000000000000, 38.59999999999999432, 2.500000000000000000 ) ) ;
#14819 = CARTESIAN_POINT ( 'NONE',  ( 3.481649420246394122, 15.87819992234354594, 1.193696214020467439 ) ) ;
#14820 = ORIENTED_EDGE ( 'NONE', *, *, #1070, .T. ) ;
#14821 = CARTESIAN_POINT ( 'NONE',  ( -4.243569643750000786, -22.60971946825739209, -8.008545724169261248 ) ) ;
#14822 = CIRCLE ( 'NONE', #6801, 0.9999999999999991118 ) ;
#14823 = CARTESIAN_POINT ( 'NONE',  ( 2.211161402132902243, 19.62180007765647360, 2.942372952327172442 ) ) ;
#14824 = CIRCLE ( 'NONE', #13919, 6.099999999999999645 ) ;
#14825 = ORIENTED_EDGE ( 'NONE', *, *, #3723, .F. ) ;
#14826 = PLANE ( 'NONE',  #7058 ) ;
#14827 = CARTESIAN_POINT ( 'NONE',  ( -8.500000000000010658, 14.99364916731036956, 22.64999999999998437 ) ) ;
#14828 = DIRECTION ( 'NONE',  ( -0.000000000000000000, 1.000000000000000000, -0.000000000000000000 ) ) ;
#14829 = DIRECTION ( 'NONE',  ( -4.915049848600951133E-16, 0.000000000000000000, -1.000000000000000000 ) ) ;
#14830 = EDGE_CURVE ( 'NONE', #8268, #2949, #15836, .T. ) ;
#14831 = CARTESIAN_POINT ( 'NONE',  ( 8.500000000000019540, 0.000000000000000000, -22.49999999999999289 ) ) ;
#14832 = CARTESIAN_POINT ( 'NONE',  ( 4.243569643750000786, -20.41578959921466918, -4.875289154763852828 ) ) ;
#14833 = ORIENTED_EDGE ( 'NONE', *, *, #12146, .F. ) ;
#14834 = CARTESIAN_POINT ( 'NONE',  ( 1.071796769724495224, -19.81246127307154836, -10.98743419085593409 ) ) ;
#14835 = EDGE_CURVE ( 'NONE', #11426, #17611, #2653, .T. ) ;
#14836 = CARTESIAN_POINT ( 'NONE',  ( -2.000000000000005773, -26.32384188007369730, -7.273385382783162711 ) ) ;
#14837 = AXIS2_PLACEMENT_3D ( 'NONE', #5772, #32, #14503 ) ;
#14838 = AXIS2_PLACEMENT_3D ( 'NONE', #15394, #16879, #17912 ) ;
#14839 = VERTEX_POINT ( 'NONE', #17057 ) ;
#14840 = ORIENTED_EDGE ( 'NONE', *, *, #11339, .F. ) ;
#14841 = DIRECTION ( 'NONE',  ( -0.000000000000000000, 1.000000000000000000, -0.000000000000000000 ) ) ;
#14842 = EDGE_CURVE ( 'NONE', #12048, #2315, #4222, .T. ) ;
#14843 = CARTESIAN_POINT ( 'NONE',  ( 1.820000000000000062, 0.000000000000000000, 0.000000000000000000 ) ) ;
#14844 = SURFACE_SIDE_STYLE ('',( #5263 ) ) ;
#14845 = CARTESIAN_POINT ( 'NONE',  ( 1.336863392178569754, 28.75319992234354771, 4.297206761780648421 ) ) ;
#14846 = CARTESIAN_POINT ( 'NONE',  ( -1.135272562821019626, 36.50319992234354061, 3.311245368580577164 ) ) ;
#14847 = EDGE_CURVE ( 'NONE', #17808, #7377, #11646, .T. ) ;
#14848 = CARTESIAN_POINT ( 'NONE',  ( 1.497042530366522461, 16.12819992234354416, 2.161531897785029965 ) ) ;
#14849 = ORIENTED_EDGE ( 'NONE', *, *, #8513, .F. ) ;
#14850 = CARTESIAN_POINT ( 'NONE',  ( 4.499999999999999112, 16.74680007765647716, -0.05647727720537982360 ) ) ;
#14851 = CARTESIAN_POINT ( 'NONE',  ( 3.999999999999996447, -24.21647428920293876, -6.276911511947378841 ) ) ;
#14852 = ORIENTED_EDGE ( 'NONE', *, *, #520, .T. ) ;
#14853 = DIRECTION ( 'NONE',  ( -0.000000000000000000, -0.5735764363510414965, -0.8191520442889950182 ) ) ;
#14854 = CARTESIAN_POINT ( 'NONE',  ( 1.027846397803542144, 38.74680007765647360, -3.346150245485522312 ) ) ;
#14855 = CARTESIAN_POINT ( 'NONE',  ( 1.475796370471763337E-14, -22.05939178977998694, -14.19638352958117267 ) ) ;
#14856 = CARTESIAN_POINT ( 'NONE',  ( 4.243569643749997233, -22.41197890986777352, -3.454652828211637772 ) ) ;
#14857 = CARTESIAN_POINT ( 'NONE',  ( -2.121784821875005722, -26.60955462421497586, -7.313667161985088150 ) ) ;
#14858 = CYLINDRICAL_SURFACE ( 'NONE', #4060, 4.000000000000000000 ) ;
#14859 = VERTEX_POINT ( 'NONE', #17431 ) ;
#14860 = EDGE_CURVE ( 'NONE', #17338, #9655, #9436, .T. ) ;
#14861 = CARTESIAN_POINT ( 'NONE',  ( 3.132887738848207260, -10.75727755901226779, 20.85177242120515473 ) ) ;
#14862 = LINE ( 'NONE', #7788, #4537 ) ;
#14863 = CARTESIAN_POINT ( 'NONE',  ( 4.000000000000000888, -22.10963251316630362, -7.294347536058173098 ) ) ;
#14864 = CARTESIAN_POINT ( 'NONE',  ( -4.243569643750005227, -28.98301395881438580, -12.83906343559744201 ) ) ;
#14865 = ORIENTED_EDGE ( 'NONE', *, *, #16477, .T. ) ;
#14866 = AXIS2_PLACEMENT_3D ( 'NONE', #13571, #7827, #4870 ) ;
#14867 = CARTESIAN_POINT ( 'NONE',  ( -3.500000000000000444, 29.50319992234354416, -0.05647727720529563400 ) ) ;
#14868 = CARTESIAN_POINT ( 'NONE',  ( 3.276967058447619152, -25.10900663730464188, -15.57833582608148326 ) ) ;
#14869 = ADVANCED_FACE ( 'NONE', ( #4698 ), #14798, .T. ) ;
#14870 = CARTESIAN_POINT ( 'NONE',  ( 4.243569643750003451, -19.90372931761987019, -8.415481395913838369 ) ) ;
#14871 = CARTESIAN_POINT ( 'NONE',  ( 2.500000000000001332, 21.74680007765648071, -0.05647727720535888202 ) ) ;
#14872 = CARTESIAN_POINT ( 'NONE',  ( -1.444289557195956863, 19.00319992234354771, 4.262301884875733471 ) ) ;
#14873 = CARTESIAN_POINT ( 'NONE',  ( 4.243569643750000786, -25.83608692273200802, -12.61627597329485440 ) ) ;
#14874 = CARTESIAN_POINT ( 'NONE',  ( -3.999999999999997335, -23.91744991381563779, -13.90249626042782793 ) ) ;
#14875 = CARTESIAN_POINT ( 'NONE',  ( 4.730628863548789710E-15, -16.85359330517172083, -8.330925841085024430 ) ) ;
#14876 = CARTESIAN_POINT ( 'NONE',  ( 0.05938372350927906274, 17.37180007765647005, 3.680117784833935701 ) ) ;
#14877 = DIRECTION ( 'NONE',  ( 0.000000000000000000, 0.000000000000000000, -1.000000000000000000 ) ) ;
#14878 = CARTESIAN_POINT ( 'NONE',  ( -6.428571428571425272, -14.26578344203648285, -2.827263138854410496 ) ) ;
#14879 = CARTESIAN_POINT ( 'NONE',  ( -8.500000000000005329, 15.00000000000000178, -18.35000000000000142 ) ) ;
#14880 = EDGE_LOOP ( 'NONE', ( #10188, #12615, #9633, #8885 ) ) ;
#14881 = ORIENTED_EDGE ( 'NONE', *, *, #2441, .F. ) ;
#14882 = CARTESIAN_POINT ( 'NONE',  ( 2.121784821875004390, -16.81387309597561242, -6.138454447673516334 ) ) ;
#14883 = AXIS2_PLACEMENT_3D ( 'NONE', #14407, #1713, #12911 ) ;
#14884 = CARTESIAN_POINT ( 'NONE',  ( -6.158835246850665095E-15, -22.31750118613795664, -14.56500194951122218 ) ) ;
#14885 = CARTESIAN_POINT ( 'NONE',  ( 7.485948097525552569, -12.69170840778861731, 7.144968677233840104 ) ) ;
#14886 = ORIENTED_EDGE ( 'NONE', *, *, #11691, .T. ) ;
#14887 = CIRCLE ( 'NONE', #15180, 2.499999999999999556 ) ;
#14888 = CARTESIAN_POINT ( 'NONE',  ( -0.8262555684460826111, 29.00319992234355482, 2.360188852285421302 ) ) ;
#14889 =( LENGTH_UNIT ( ) NAMED_UNIT ( * ) SI_UNIT ( .MILLI., .METRE. ) );
#14890 = CARTESIAN_POINT ( 'NONE',  ( -4.243569643750005227, -27.66020330247980041, -10.94989403345594425 ) ) ;
#14891 = CARTESIAN_POINT ( 'NONE',  ( 3.500000000000000444, 24.24680007765647716, -0.05647727720536935281 ) ) ;
#14892 = AXIS2_PLACEMENT_3D ( 'NONE', #3032, #15732, #8664 ) ;
#14893 = CARTESIAN_POINT ( 'NONE',  ( -5.577813053751546416E-15, -23.57947491511155036, -2.419712850136908511 ) ) ;
#14894 = CARTESIAN_POINT ( 'NONE',  ( 1.598251304517956273, -15.40332308709066211, -10.50456014341326849 ) ) ;
#14895 = AXIS2_PLACEMENT_3D ( 'NONE', #16634, #11041, #2801 ) ;
#14896 = CARTESIAN_POINT ( 'NONE',  ( -4.243569643749997233, -23.97970686843945742, -14.23658061064251257 ) ) ;
#14897 = EDGE_CURVE ( 'NONE', #6273, #1346, #9147, .T. ) ;
#14898 = AXIS2_PLACEMENT_3D ( 'NONE', #151, #8480, #15472 ) ;
#14899 = EDGE_CURVE ( 'NONE', #1204, #7975, #18360, .T. ) ;
#14900 = DIRECTION ( 'NONE',  ( 0.000000000000000000, 0.000000000000000000, -1.000000000000000000 ) ) ;
#14901 = EDGE_CURVE ( 'NONE', #8582, #16215, #14497, .T. ) ;
#14902 = CARTESIAN_POINT ( 'NONE',  ( -2.000000000000005773, -29.09851789021691815, -11.23603339602441054 ) ) ;
#14903 = CARTESIAN_POINT ( 'NONE',  ( 0.000000000000000000, 25.39999999999999503, 2.500000000000000000 ) ) ;
#14904 = CARTESIAN_POINT ( 'NONE',  ( 4.243569643750000786, -23.99705747368147968, -9.989869731293264721 ) ) ;
#14905 = VERTEX_POINT ( 'NONE', #2301 ) ;
#14906 = FACE_OUTER_BOUND ( 'NONE', #9409, .T. ) ;
#14907 = DIRECTION ( 'NONE',  ( 0.000000000000000000, 0.000000000000000000, -1.000000000000000000 ) ) ;
#14908 = EDGE_CURVE ( 'NONE', #1717, #3078, #3533, .T. ) ;
#14909 = CARTESIAN_POINT ( 'NONE',  ( 2.518350579753628971, 26.87180007765648426, 0.7558219633769073242 ) ) ;
#14910 = ORIENTED_EDGE ( 'NONE', *, *, #15287, .F. ) ;
#14911 = CARTESIAN_POINT ( 'NONE',  ( -2.864755990943265829, 33.24680007765648071, -2.011557305968488141 ) ) ;
#14912 = CARTESIAN_POINT ( 'NONE',  ( -1.734723475976807094E-15, 31.99999999999999289, -12.50000000000000000 ) ) ;
#14913 = AXIS2_PLACEMENT_3D ( 'NONE', #10835, #12586, #6751 ) ;
#14914 = AXIS2_PLACEMENT_3D ( 'NONE', #10668, #16436, #7795 ) ;
#14915 = ITEM_DEFINED_TRANSFORMATION ( 'NONE', 'NONE', #5092,  #16940 ) ;
#14916 = CIRCLE ( 'NONE', #3635, 2.200000000000000622 ) ;
#14917 = CARTESIAN_POINT ( 'NONE',  ( 8.499999999999994671, 15.00000000000000178, 18.35000000000000142 ) ) ;
#14918 =( BOUNDED_CURVE ( )  B_SPLINE_CURVE ( 2, ( #9742, #12706, #5303, #5394, #14014, #10955, #11306, #16639, #4273 ),
 .UNSPECIFIED., .F., .F. ) 
 B_SPLINE_CURVE_WITH_KNOTS ( ( 3, 2, 2, 2, 3 ),
 ( 0.4913793103448276245, 0.4942528735632183978, 0.5000000000000000000, 0.5057471264367816577, 0.5086206896551724865 ),
 .UNSPECIFIED. ) 
 CURVE ( )  GEOMETRIC_REPRESENTATION_ITEM ( )  RATIONAL_B_SPLINE_CURVE ( ( 0.9330127018922194093, 0.9330127018922200755, 1.000000000000000000, 0.8660254037844387076, 1.000000000000000000, 0.8660254037844387076, 1.000000000000000000, 0.9330127018922180770, 0.9330127018922194093 ) ) 
 REPRESENTATION_ITEM ( '' )  );
#14919 = ORIENTED_EDGE ( 'NONE', *, *, #10738, .F. ) ;
#14920 = CARTESIAN_POINT ( 'NONE',  ( 4.243569643750000786, -22.22255537372044998, -7.455618094274186092 ) ) ;
#14921 = CARTESIAN_POINT ( 'NONE',  ( -2.115076519116362519, 20.12180007765648071, 3.012182706137107147 ) ) ;
#14922 = ORIENTED_EDGE ( 'NONE', *, *, #4423, .T. ) ;
#14923 = CARTESIAN_POINT ( 'NONE',  ( -1.734723475976807094E-15, 23.19999999999999574, -2.500000000000000000 ) ) ;
#14924 = FACE_OUTER_BOUND ( 'NONE', #775, .T. ) ;
#14925 = CARTESIAN_POINT ( 'NONE',  ( -14.99999999999999645, -10.00000000000000000, 30.00000000000000000 ) ) ;
#14926 = CIRCLE ( 'NONE', #11044, 0.5000000000000026645 ) ;
#14927 = CARTESIAN_POINT ( 'NONE',  ( 9.985555166373632829, -9.918630114099121542, 7.321306590882093346 ) ) ;
#14928 = VECTOR ( 'NONE', #11312, 1000.000000000000000 ) ;
#14929 = CARTESIAN_POINT ( 'NONE',  ( -1.071796769724486786, -18.49886088984402832, -9.111418421893864306 ) ) ;
#14930 = CARTESIAN_POINT ( 'NONE',  ( -2.121784821874996396, -23.99791796127240318, -16.39833380239318217 ) ) ;
#14931 = ORIENTED_EDGE ( 'NONE', *, *, #10461, .T. ) ;
#14932 = CYLINDRICAL_SURFACE ( 'NONE', #12157, 4.000000000000000000 ) ;
#14933 = CARTESIAN_POINT ( 'NONE',  ( -3.999999999999997335, -21.65899269638835278, -10.67708508704667913 ) ) ;
#14934 = ORIENTED_EDGE ( 'NONE', *, *, #7209, .F. ) ;
#14935 = EDGE_LOOP ( 'NONE', ( #810, #4667 ) ) ;
#14936 = CARTESIAN_POINT ( 'NONE',  ( 8.500000000000019540, 10.00000000000000000, 20.49999999999998934 ) ) ;
#14937 = PRODUCT_CONTEXT ( 'NONE', #7236, 'mechanical' ) ;
#14938 = CARTESIAN_POINT ( 'NONE',  ( 4.518350579753602325, 35.62819992234354771, -1.405661355842793725 ) ) ;
#14939 = CARTESIAN_POINT ( 'NONE',  ( -3.500000000000000444, 34.50319992234354771, -0.05647727720529563400 ) ) ;
#14940 = CARTESIAN_POINT ( 'NONE',  ( 0.8262555684460829442, 17.75319992234354061, -2.360188852285421302 ) ) ;
#14941 = AXIS2_PLACEMENT_3D ( 'NONE', #7723, #6347, #17683 ) ;
#14942 = VERTEX_POINT ( 'NONE', #9149 ) ;
#14943 = CARTESIAN_POINT ( 'NONE',  ( -4.499999999999999112, 17.99680007765647005, 0.05647727720537927543 ) ) ;
#14944 = CARTESIAN_POINT ( 'NONE',  ( -5.279047395330986450E-15, -24.86069615324935356, -3.170637775906417488 ) ) ;
#14945 = ORIENTED_EDGE ( 'NONE', *, *, #18083, .F. ) ;
#14946 = DIRECTION ( 'NONE',  ( -0.000000000000000000, -1.000000000000000000, -0.000000000000000000 ) ) ;
#14947 = CARTESIAN_POINT ( 'NONE',  ( 2.211161402132902243, 34.62180007765648071, 2.942372952327172442 ) ) ;
#14948 = DIRECTION ( 'NONE',  ( -1.000000000000000000, -0.000000000000000000, -0.000000000000000000 ) ) ;
#14949 = FACE_OUTER_BOUND ( 'NONE', #5231, .T. ) ;
#14950 = CARTESIAN_POINT ( 'NONE',  ( 2.121784821875004390, -21.75021530132177006, -13.18828172883567973 ) ) ;
#14951 = ADVANCED_FACE ( 'NONE', ( #636 ), #7655, .F. ) ;
#14952 = CARTESIAN_POINT ( 'NONE',  ( 3.082316921986471225, -29.06618978543598786, -12.78463801463987437 ) ) ;
#14953 = ORIENTED_EDGE ( 'NONE', *, *, #6552, .T. ) ;
#14954 = CARTESIAN_POINT ( 'NONE',  ( -5.526342620816817153, -10.00000000000000178, 19.09106094340727111 ) ) ;
#14955 = SURFACE_SIDE_STYLE ('',( #12138 ) ) ;
#14956 = CARTESIAN_POINT ( 'NONE',  ( 2.121784821875004390, -23.81509047218551700, -16.13722908827605806 ) ) ;
#14957 = ORIENTED_EDGE ( 'NONE', *, *, #10461, .F. ) ;
#14958 = CARTESIAN_POINT ( 'NONE',  ( 1.027846397803612311, 23.75319992234354416, 3.346150245485499219 ) ) ;
#14959 = CARTESIAN_POINT ( 'NONE',  ( 0.000000000000000000, 27.59999999999999432, 2.500000000000000000 ) ) ;
#14960 = CARTESIAN_POINT ( 'NONE',  ( -4.243569643750005227, -21.72368718624651507, -2.471670375064849434 ) ) ;
#14961 = CARTESIAN_POINT ( 'NONE',  ( 0.8262555684461332373, 22.24680007765648071, 2.360188852285403982 ) ) ;
#14962 = CARTESIAN_POINT ( 'NONE',  ( -2.829195390882724315, 16.62819992234354061, 3.793023760679264722 ) ) ;
#14963 = CARTESIAN_POINT ( 'NONE',  ( 4.000000000000003553, -24.00348637926829909, -14.02536906707117659 ) ) ;
#14964 = ORIENTED_EDGE ( 'NONE', *, *, #2817, .F. ) ;
#14965 = CARTESIAN_POINT ( 'NONE',  ( -5.330712181944245322E-15, -25.01042347868947857, -2.894126148162874834 ) ) ;
#14966 = CARTESIAN_POINT ( 'NONE',  ( -3.481649420246369697, 17.87180007765648071, 1.193696214020542490 ) ) ;
#14967 = ADVANCED_FACE ( 'NONE', ( #1942 ), #13592, .F. ) ;
#14968 = CARTESIAN_POINT ( 'NONE',  ( 0.000000000000000000, 9.254131787996968228, 30.52396275209373044 ) ) ;
#14969 = CARTESIAN_POINT ( 'NONE',  ( 0.000000000000000000, 49.00000000000000000, 0.000000000000000000 ) ) ;
#14970 = CARTESIAN_POINT ( 'NONE',  ( -1.734723475976807094E-15, 31.99999999999999289, -10.50000000000000178 ) ) ;
#14971 = ORIENTED_EDGE ( 'NONE', *, *, #9098, .F. ) ;
#14972 = ORIENTED_EDGE ( 'NONE', *, *, #14791, .F. ) ;
#14973 = FACE_OUTER_BOUND ( 'NONE', #2237, .T. ) ;
#14974 = CARTESIAN_POINT ( 'NONE',  ( 0.000000000000000000, 5.977523610840987267, 32.81826849749789687 ) ) ;
#14975 = ORIENTED_EDGE ( 'NONE', *, *, #4953, .F. ) ;
#14976 = CARTESIAN_POINT ( 'NONE',  ( 2.500000000000001332, 28.25319992234354771, 0.05647727720530566764 ) ) ;
#14977 = CARTESIAN_POINT ( 'NONE',  ( 4.243569643750000786, -23.99705747368147968, -9.989869731293264721 ) ) ;
#14978 = CARTESIAN_POINT ( 'NONE',  ( 2.115076519116362963, 21.37180007765648071, -3.012182706137107147 ) ) ;
#14979 = CARTESIAN_POINT ( 'NONE',  ( 0.9009826423167504039, -10.00000000000000178, -12.54001985818112352 ) ) ;
#14980 = CARTESIAN_POINT ( 'NONE',  ( -5.330712181944245322E-15, -28.88206442405900631, -8.423402447113588210 ) ) ;
#14981 = PLANE ( 'NONE',  #15029 ) ;
#14982 = CARTESIAN_POINT ( 'NONE',  ( 1.336863392178479160, 21.24680007765647716, -4.297206761780677731 ) ) ;
#14983 = CARTESIAN_POINT ( 'NONE',  ( -5.577813053751546416E-15, -29.51599103134483570, -10.89793650852800511 ) ) ;
#14984 = DIRECTION ( 'NONE',  ( 0.000000000000000000, 1.000000000000000000, 0.000000000000000000 ) ) ;
#14985 = CARTESIAN_POINT ( 'NONE',  ( -4.243569643749997233, -21.62445862667299323, -10.87293752878082742 ) ) ;
#14986 = CIRCLE ( 'NONE', #10519, 2.149999999999995470 ) ;
#14987 = DIRECTION ( 'NONE',  ( 0.000000000000000000, 1.000000000000000000, 1.224646799147353454E-16 ) ) ;
#14988 = CARTESIAN_POINT ( 'NONE',  ( -8.000000000000003553, 16.59999999999999787, -2.500000000000001776 ) ) ;
#14989 = CARTESIAN_POINT ( 'NONE',  ( 2.518350579753628971, 34.37180007765647360, 0.7558219633769073242 ) ) ;
#14990 = ORIENTED_EDGE ( 'NONE', *, *, #18293, .F. ) ;
#14991 = CARTESIAN_POINT ( 'NONE',  ( -0.05938372350927861865, 33.62180007765648071, -3.680117784833935701 ) ) ;
#14992 = DIRECTION ( 'NONE',  ( -1.000000000000000000, -0.000000000000000000, -0.000000000000000000 ) ) ;
#14993 = EDGE_CURVE ( 'NONE', #10845, #1108, #5882, .T. ) ;
#14994 = APPLICATION_PROTOCOL_DEFINITION ( 'draft international standard', 'automotive_design', 1998, #14235 ) ;
#14995 = FACE_OUTER_BOUND ( 'NONE', #4385, .T. ) ;
#14996 = ADVANCED_FACE ( 'NONE', ( #4972 ), #14826, .T. ) ;
#14997 = VERTEX_POINT ( 'NONE', #3501 ) ;
#14998 = CARTESIAN_POINT ( 'NONE',  ( 4.243569643749997233, -25.02533654799221452, -7.186914330003371099 ) ) ;
#14999 = CARTESIAN_POINT ( 'NONE',  ( 2.115076519116362963, 23.87180007765647005, -3.012182706137107147 ) ) ;
#15000 = ORIENTED_EDGE ( 'NONE', *, *, #11021, .T. ) ;
#15001 = AXIS2_PLACEMENT_3D ( 'NONE', #14118, #1430, #15790 ) ;
#15002 = EDGE_CURVE ( 'NONE', #526, #3808, #7754, .T. ) ;
#15003 = FACE_OUTER_BOUND ( 'NONE', #15022, .T. ) ;
#15004 = AXIS2_PLACEMENT_3D ( 'NONE', #8236, #11102, #16790 ) ;
#15005 = CARTESIAN_POINT ( 'NONE',  ( 14.99999999999999822, 13.00000000000000178, 24.99999999999999645 ) ) ;
#15006 = CARTESIAN_POINT ( 'NONE',  ( -3.792279431941310452, -28.18008910945223278, -13.57208143547394918 ) ) ;
#15007 = CARTESIAN_POINT ( 'NONE',  ( 4.299564228933482956E-15, -19.02660638327879994, -9.865117096409875330 ) ) ;
#15008 = CARTESIAN_POINT ( 'NONE',  ( -1.661723472263481630E-14, -21.28506360070608139, -13.09052826979102946 ) ) ;
#15009 = CARTESIAN_POINT ( 'NONE',  ( 2.121784821874994176, -22.69489544611912279, -1.722954459712693787 ) ) ;
#15010 = ORIENTED_EDGE ( 'NONE', *, *, #14355, .T. ) ;
#15011 = FACE_OUTER_BOUND ( 'NONE', #5460, .T. ) ;
#15012 = CARTESIAN_POINT ( 'NONE',  ( 3.999999999999996447, -24.53911103535534366, -6.737684537866704737 ) ) ;
#15013 = CARTESIAN_POINT ( 'NONE',  ( 3.518350579753631191, 29.37180007765647005, 1.080741659609802285 ) ) ;
#15014 = ORIENTED_EDGE ( 'NONE', *, *, #17032, .T. ) ;
#15015 = ORIENTED_EDGE ( 'NONE', *, *, #4450, .T. ) ;
#15016 =( BOUNDED_CURVE ( )  B_SPLINE_CURVE ( 2, ( #15443, #18234, #14219, #2911, #8287, #9939, #16931, #15528, #5686 ),
 .UNSPECIFIED., .F., .T. ) 
 B_SPLINE_CURVE_WITH_KNOTS ( ( 3, 2, 2, 2, 3 ),
 ( 0.8017241379310344751, 0.8045977011494253039, 0.8103448275862068506, 0.8160919540229885083, 0.8189655172413793371 ),
 .UNSPECIFIED. ) 
 CURVE ( )  GEOMETRIC_REPRESENTATION_ITEM ( )  RATIONAL_B_SPLINE_CURVE ( ( 0.9330127018922194093, 0.9330127018922194093, 1.000000000000000000, 0.8660254037844387076, 1.000000000000000000, 0.8660254037844387076, 1.000000000000000000, 0.9330127018922194093, 0.9330127018922194093 ) ) 
 REPRESENTATION_ITEM ( '' )  );
#15017 = CARTESIAN_POINT ( 'NONE',  ( -4.648177544792955347E-16, -29.58051838113927090, -10.99009111451728415 ) ) ;
#15018 = CARTESIAN_POINT ( 'NONE',  ( 1.444289557195957086, 30.25319992234354061, -4.262301884875733471 ) ) ;
#15019 = CARTESIAN_POINT ( 'NONE',  ( 3.518350579753606322, 35.62819992234354061, -1.080741659609876892 ) ) ;
#15020 = CIRCLE ( 'NONE', #4326, 8.000000000000003553 ) ;
#15021 = CARTESIAN_POINT ( 'NONE',  ( 1.497042530366522461, 26.12819992234354416, 2.161531897785029965 ) ) ;
#15022 = EDGE_LOOP ( 'NONE', ( #12983, #2761, #7373, #10828 ) ) ;
#15023 = CARTESIAN_POINT ( 'NONE',  ( 4.499999999999999112, 26.74680007765647360, -0.05647727720537982360 ) ) ;
#15024 = CARTESIAN_POINT ( 'NONE',  ( 3.999999999999996447, -23.18403670377106351, -4.802437832227187897 ) ) ;
#15025 = ORIENTED_EDGE ( 'NONE', *, *, #5346, .F. ) ;
#15026 = LINE ( 'NONE', #3787, #14499 ) ;
#15027 = CARTESIAN_POINT ( 'NONE',  ( 3.064183985264992582, -21.85725672082847382, -2.451266466499125052 ) ) ;
#15028 = CARTESIAN_POINT ( 'NONE',  ( 4.243569643749997233, -22.15386951350980382, -3.086034408281590480 ) ) ;
#15029 = AXIS2_PLACEMENT_3D ( 'NONE', #2375, #12177, #10515 ) ;
#15030 = CARTESIAN_POINT ( 'NONE',  ( 2.121784821874994176, -26.82464578784662379, -7.620849178593458007 ) ) ;
#15031 = ADVANCED_FACE ( 'NONE', ( #9415 ), #877, .T. ) ;
#15032 = CARTESIAN_POINT ( 'NONE',  ( -9.000000000000003553, 43.00000000000000000, -2.500000000000001776 ) ) ;
#15033 = VERTEX_POINT ( 'NONE', #9241 ) ;
#15034 = CARTESIAN_POINT ( 'NONE',  ( -3.544496300715703541, -10.00000000000000178, 23.01862375599376875 ) ) ;
#15035 = CARTESIAN_POINT ( 'NONE',  ( 8.500000000000019540, 10.00000000000000000, 22.49999999999999289 ) ) ;
#15036 =( NAMED_UNIT ( * ) SI_UNIT ( $, .STERADIAN. ) SOLID_ANGLE_UNIT ( ) );
#15037 = CARTESIAN_POINT ( 'NONE',  ( -2.000000000000005773, -25.54951369099979175, -6.167530122993019503 ) ) ;
#15038 = ORIENTED_EDGE ( 'NONE', *, *, #11307, .T. ) ;
#15039 = CARTESIAN_POINT ( 'NONE',  ( 0.05938372350920109732, 32.62819992234354771, -3.680117784833935701 ) ) ;
#15040 = CARTESIAN_POINT ( 'NONE',  ( 1.135272562821020070, 15.25319992234354594, -3.311245368580577164 ) ) ;
#15041 = CARTESIAN_POINT ( 'NONE',  ( 2.769796424106844235, -22.34959361326263760, -1.882087514909482229 ) ) ;
#15042 = CARTESIAN_POINT ( 'NONE',  ( 2.055738996568313048, 29.49680007765648426, 1.423772053676023441 ) ) ;
#15043 = AXIS2_PLACEMENT_3D ( 'NONE', #5776, #15446, #10028 ) ;
#15044 = CARTESIAN_POINT ( 'NONE',  ( 4.518350579753602325, 15.62819992234354238, -1.405661355842793725 ) ) ;
#15045 = CARTESIAN_POINT ( 'NONE',  ( -4.000000000000004441, -27.14171411459323835, -10.45458693782125792 ) ) ;
#15046 = ORIENTED_EDGE ( 'NONE', *, *, #10144, .T. ) ;
#15047 = CARTESIAN_POINT ( 'NONE',  ( -5.330712181944245322E-15, -24.23609528961556947, -1.788270888372730960 ) ) ;
#15048 = CARTESIAN_POINT ( 'NONE',  ( 1.336863392178479160, 38.74680007765646650, -4.297206761780677731 ) ) ;
#15049 = AXIS2_PLACEMENT_3D ( 'NONE', #11155, #9771, #12277 ) ;
#15050 = CARTESIAN_POINT ( 'NONE',  ( -5.577813053751546416E-15, -28.74166284227092305, -9.792081248737861898 ) ) ;
#15051 = CARTESIAN_POINT ( 'NONE',  ( 1.071796769724495224, -21.03848090506694390, -12.73837168451689550 ) ) ;
#15052=STYLED_ITEM('',(#18396),#14274);
#15053 = CYLINDRICAL_SURFACE ( 'NONE', #7937, 0.9999999999999991118 ) ;
#15054 = ORIENTED_EDGE ( 'NONE', *, *, #18293, .T. ) ;
#15055 = AXIS2_PLACEMENT_3D ( 'NONE', #14424, #7458, #3209 ) ;
#15056 = ORIENTED_EDGE ( 'NONE', *, *, #2770, .F. ) ;
#15057 = CARTESIAN_POINT ( 'NONE',  ( 3.481649420246369697, 16.62180007765648071, -1.193696214020541824 ) ) ;
#15058 = ADVANCED_FACE ( 'NONE', ( #14924 ), #2217, .F. ) ;
#15059 = FACE_OUTER_BOUND ( 'NONE', #13509, .T. ) ;
#15060 = DIRECTION ( 'NONE',  ( 0.000000000000000000, 0.000000000000000000, 1.000000000000000000 ) ) ;
#15061 = ORIENTED_EDGE ( 'NONE', *, *, #15940, .T. ) ;
#15062 = CARTESIAN_POINT ( 'NONE',  ( -3.500000000000000444, 14.50319992234354416, -0.05647727720529563400 ) ) ;
#15063 = CARTESIAN_POINT ( 'NONE',  ( 2.121784821875004390, -20.68551404134514016, -11.66773074662423149 ) ) ;
#15064 = CARTESIAN_POINT ( 'NONE',  ( -2.115076519116362519, 25.12180007765647360, 3.012182706137107147 ) ) ;
#15065 = ADVANCED_FACE ( 'NONE', ( #2124 ), #10812, .T. ) ;
#15066 = DIRECTION ( 'NONE',  ( 0.000000000000000000, 0.000000000000000000, 1.000000000000000000 ) ) ;
#15067 = ADVANCED_FACE ( 'NONE', ( #17803 ), #5064, .T. ) ;
#15068 = DIRECTION ( 'NONE',  ( -0.000000000000000000, 0.000000000000000000, 1.000000000000000000 ) ) ;
#15069 = CARTESIAN_POINT ( 'NONE',  ( 4.730628863548789710E-15, -21.24145304325719152, -14.59743897989583594 ) ) ;
#15070 = CARTESIAN_POINT ( 'NONE',  ( 0.000000000000000000, 16.59999999999999787, 2.500000000000000000 ) ) ;
#15071 = CARTESIAN_POINT ( 'NONE',  ( -3.607379964056306676, 20.24680007765648071, 2.690724712371306282 ) ) ;
#15072 = CARTESIAN_POINT ( 'NONE',  ( -2.000000000000005773, -22.96841972742010540, -2.481345923692543920 ) ) ;
#15073 = CARTESIAN_POINT ( 'NONE',  ( 8.000000000000000000, 23.19999999999999574, -2.500000000000000888 ) ) ;
#15074 = CARTESIAN_POINT ( 'NONE',  ( -2.121784821875005722, -25.54485336423835307, -5.793116179773641683 ) ) ;
#15075 = FACE_OUTER_BOUND ( 'NONE', #17443, .T. ) ;
#15076 = LINE ( 'NONE', #13857, #4654 ) ;
#15077 = AXIS2_PLACEMENT_3D ( 'NONE', #11454, #11550, #3044 ) ;
#15078 = CARTESIAN_POINT ( 'NONE',  ( -1.497042530366477164, 40.12180007765647360, 2.161531897785062384 ) ) ;
#15079 = AXIS2_PLACEMENT_3D ( 'NONE', #5461, #11106, #16886 ) ;
#15080 = DIRECTION ( 'NONE',  ( -0.000000000000000000, -1.000000000000000000, -0.000000000000000000 ) ) ;
#15081 = CARTESIAN_POINT ( 'NONE',  ( -2.211161402132901799, 30.87180007765647716, -2.942372952327172886 ) ) ;
#15082 = DIRECTION ( 'NONE',  ( -0.5000000000000042188, 0.000000000000000000, 0.8660254037844361541 ) ) ;
#15083 = DIRECTION ( 'NONE',  ( -0.000000000000000000, -0.5735764363510414965, -0.8191520442889950182 ) ) ;
#15084 = EDGE_LOOP ( 'NONE', ( #3483, #14356, #5061, #15842 ) ) ;
#15085 = CARTESIAN_POINT ( 'NONE',  ( -4.243569643750004339, -23.30460723893907371, -4.729458197136390929 ) ) ;
#15086 = CARTESIAN_POINT ( 'NONE',  ( 3.518350579753631191, 24.37180007765648071, 1.080741659609802285 ) ) ;
#15087 = AXIS2_PLACEMENT_3D ( 'NONE', #11613, #1441, #15534 ) ;
#15088 = ORIENTED_EDGE ( 'NONE', *, *, #4624, .F. ) ;
#15089 = PRODUCT_DEFINITION_SHAPE ( 'NONE', 'NONE',  #18373 ) ;
#15090 = VECTOR ( 'NONE', #7379, 1000.000000000000000 ) ;
#15091 = DIRECTION ( 'NONE',  ( -1.000000000000000000, 0.000000000000000000, 4.336808689942021680E-16 ) ) ;
#15092 = VECTOR ( 'NONE', #13437, 1000.000000000000000 ) ;
#15093 = CARTESIAN_POINT ( 'NONE',  ( 4.243569643749997233, -28.86471381881699116, -12.67011332646283073 ) ) ;
#15094 = DIRECTION ( 'NONE',  ( 0.000000000000000000, 0.000000000000000000, 1.000000000000000000 ) ) ;
#15095 = CARTESIAN_POINT ( 'NONE',  ( 7.035635943437157813, -13.82009150476320869, -0.02313312325170999509 ) ) ;
#15096 = DIRECTION ( 'NONE',  ( -1.000000000000000000, 0.000000000000000000, 0.000000000000000000 ) ) ;
#15097 = CARTESIAN_POINT ( 'NONE',  ( 4.730628863548789710E-15, -21.98351755778634953, -15.65721693719472185 ) ) ;
#15098 = ADVANCED_FACE ( 'NONE', ( #16487 ), #3765, .F. ) ;
#15099 = ORIENTED_EDGE ( 'NONE', *, *, #9170, .T. ) ;
#15100 = CARTESIAN_POINT ( 'NONE',  ( 3.999999999999996447, -24.02289224263940781, -6.000447698006609265 ) ) ;
#15101 = CARTESIAN_POINT ( 'NONE',  ( 2.211161402132902243, 34.62180007765648071, 2.942372952327172442 ) ) ;
#15102 = VERTEX_POINT ( 'NONE', #10445 ) ;
#15103 = EDGE_LOOP ( 'NONE', ( #2807, #1802, #16952, #6016 ) ) ;
#15104 = CARTESIAN_POINT ( 'NONE',  ( 2.000000000000004441, -19.48709775713304637, -9.588456612235146892 ) ) ;
#15105 = CIRCLE ( 'NONE', #3254, 2.200000000000000178 ) ;
#15106 = CARTESIAN_POINT ( 'NONE',  ( -1.444289557195956863, 34.00319992234354771, 4.262301884875733471 ) ) ;
#15107 = CARTESIAN_POINT ( 'NONE',  ( 10.00000000000000000, 25.39999999999999503, -2.500000000000003109 ) ) ;
#15108 = CARTESIAN_POINT ( 'NONE',  ( 2.481649420246391902, 28.37819992234355126, 0.8687765177875720335 ) ) ;
#15109 = ORIENTED_EDGE ( 'NONE', *, *, #9303, .T. ) ;
#15110 = CARTESIAN_POINT ( 'NONE',  ( 1.336863392178479160, 28.74680007765647360, -4.297206761780677731 ) ) ;
#15111 = CARTESIAN_POINT ( 'NONE',  ( -3.999999999999997335, -18.23904319394032569, -5.792891021966779519 ) ) ;
#15112 = ORIENTED_EDGE ( 'NONE', *, *, #10152, .F. ) ;
#15113 = CARTESIAN_POINT ( 'NONE',  ( 0.05938372350927906274, 34.87180007765645939, 3.680117784833935701 ) ) ;
#15114 = ADVANCED_FACE ( 'NONE', ( #16122 ), #3413, .F. ) ;
#15115 = CARTESIAN_POINT ( 'NONE',  ( -13.00000000000000178, 15.00000000000000178, 25.00000000000000355 ) ) ;
#15116 = EDGE_CURVE ( 'NONE', #9924, #1959, #16567, .T. ) ;
#15117 = AXIS2_PLACEMENT_3D ( 'NONE', #11626, #14619, #1922 ) ;
#15118 = CARTESIAN_POINT ( 'NONE',  ( -2.121784821875005722, -23.73808758973257227, -3.212787240263307531 ) ) ;
#15120 = ADVANCED_FACE ( 'NONE', ( #13684 ), #8385, .F. ) ;
#15119 = CIRCLE ( 'NONE', #12732, 0.9999999999999991118 ) ;
#15121 =( BOUNDED_CURVE ( )  B_SPLINE_CURVE ( 2, ( #9878, #11269, #9792, #16957, #11178, #8399, #4505, #2768, #7369 ),
 .UNSPECIFIED., .F., .T. ) 
 B_SPLINE_CURVE_WITH_KNOTS ( ( 3, 2, 2, 2, 3 ),
 ( 0.6293103448275861878, 0.6321839080459770166, 0.6379310344827586743, 0.6436781609195402210, 0.6465517241379310498 ),
 .UNSPECIFIED. ) 
 CURVE ( )  GEOMETRIC_REPRESENTATION_ITEM ( )  RATIONAL_B_SPLINE_CURVE ( ( 0.9330127018922194093, 0.9330127018922194093, 1.000000000000000000, 0.8660254037844387076, 1.000000000000000000, 0.8660254037844387076, 1.000000000000000000, 0.9330127018922194093, 0.9330127018922194093 ) ) 
 REPRESENTATION_ITEM ( '' )  );
#15122 = CARTESIAN_POINT ( 'NONE',  ( 4.243569643749996345, -26.05777413342408622, -8.661388009723561154 ) ) ;
#15123 = DIRECTION ( 'NONE',  ( -0.000000000000000000, -1.000000000000000000, -0.000000000000000000 ) ) ;
#15124 = ORIENTED_EDGE ( 'NONE', *, *, #9077, .F. ) ;
#15125 = CARTESIAN_POINT ( 'NONE',  ( 4.299564228933482956E-15, -18.51038759056286054, -9.127880256549779858 ) ) ;
#15126 = CARTESIAN_POINT ( 'NONE',  ( 2.021687836487040535, 2.655529440325959183E-32, -2.168404344971008868E-16 ) ) ;
#15127 = SURFACE_STYLE_USAGE ( .BOTH. , #5008 ) ;
#15128 = ORIENTED_EDGE ( 'NONE', *, *, #13288, .F. ) ;
#15129 = CARTESIAN_POINT ( 'NONE',  ( 3.518350579753605434, 33.12819992234354771, -1.080741659609877114 ) ) ;
#15130 = CARTESIAN_POINT ( 'NONE',  ( 3.500000000000000444, 18.25319992234354771, 0.05647727720529520379 ) ) ;
#15131 = CARTESIAN_POINT ( 'NONE',  ( 4.000000000000003553, -25.10045131449460598, -15.59199735278064125 ) ) ;
#15132 = CARTESIAN_POINT ( 'NONE',  ( -2.518350579753628526, 33.12180007765648071, -0.7558219633769075463 ) ) ;
#15133 = AXIS2_PLACEMENT_3D ( 'NONE', #4002, #2536, #9469 ) ;
#15134 = CARTESIAN_POINT ( 'NONE',  ( -0.05938372350918959958, 28.87819992234354416, 4.731580009072201776 ) ) ;
#15135 = CARTESIAN_POINT ( 'NONE',  ( 3.999999999999996447, -26.28134946006668571, -9.225858871387760729 ) ) ;
#15136 = VERTEX_POINT ( 'NONE', #11258 ) ;
#15137 = CARTESIAN_POINT ( 'NONE',  ( -2.121784821874996396, -17.57744672686793308, -7.228950606633243403 ) ) ;
#15138 = CARTESIAN_POINT ( 'NONE',  ( 2.864755990943265829, 16.99680007765647716, 2.011557305968487697 ) ) ;
#15139 = CARTESIAN_POINT ( 'NONE',  ( 4.243569643749997233, -25.76740106252136542, -8.246692287302257895 ) ) ;
#15140 = CARTESIAN_POINT ( 'NONE',  ( -1.071796769724496334, -29.26940833570569822, -10.54577992325387292 ) ) ;
#15141 = VECTOR ( 'NONE', #13206, 1000.000000000000000 ) ;
#15142 = DIRECTION ( 'NONE',  ( 0.000000000000000000, 0.000000000000000000, 1.000000000000000000 ) ) ;
#15143 = CARTESIAN_POINT ( 'NONE',  ( 4.299564228933482956E-15, -19.28471577963676964, -10.23373551633992307 ) ) ;
#15144 = VERTEX_POINT ( 'NONE', #6906 ) ;
#15145 = ORIENTED_EDGE ( 'NONE', *, *, #14184, .T. ) ;
#15146 = FACE_OUTER_BOUND ( 'NONE', #13095, .T. ) ;
#15147 = DIRECTION ( 'NONE',  ( 3.469446951953612217E-16, -0.000000000000000000, 1.000000000000000000 ) ) ;
#15149 = ADVANCED_FACE ( 'NONE', ( #6727, #18163 ), #13959, .T. ) ;
#15148 = DIRECTION ( 'NONE',  ( 0.000000000000000000, 0.000000000000000000, -1.000000000000000000 ) ) ;
#15150 = FACE_OUTER_BOUND ( 'NONE', #1688, .T. ) ;
#15151 = ORIENTED_EDGE ( 'NONE', *, *, #17634, .T. ) ;
#15152 = CARTESIAN_POINT ( 'NONE',  ( -2.500000000000001332, 37.00319992234354771, -0.05647727720530596601 ) ) ;
#15153 = CARTESIAN_POINT ( 'NONE',  ( -5.330712181944245322E-15, -27.55925376772441382, -6.534233044972094895 ) ) ;
#15154 = CARTESIAN_POINT ( 'NONE',  ( -1.135272562821090014, 30.99680007765647716, -3.311245368580554072 ) ) ;
#15155 = CARTESIAN_POINT ( 'NONE',  ( 2.211161402132839626, 22.87819992234354416, -2.942372952327218183 ) ) ;
#15156 = CARTESIAN_POINT ( 'NONE',  ( -1.734723475976807094E-15, 20.99999999999999289, -10.50000000000000178 ) ) ;
#15157 = FACE_OUTER_BOUND ( 'NONE', #5347, .T. ) ;
#15158 =( GEOMETRIC_REPRESENTATION_CONTEXT ( 3 ) GLOBAL_UNCERTAINTY_ASSIGNED_CONTEXT ( ( #1224 ) ) GLOBAL_UNIT_ASSIGNED_CONTEXT ( ( #9211, #11379, #14082 ) ) REPRESENTATION_CONTEXT ( 'NONE', 'WORKASPACE' ) );
#15159 = CARTESIAN_POINT ( 'NONE',  ( -2.121784821874996396, -21.19097827587949467, -12.38960848565391260 ) ) ;
#15160 = DIRECTION ( 'NONE',  ( -1.000000000000000000, -0.000000000000000000, -0.000000000000000000 ) ) ;
#15161 = ADVANCED_FACE ( 'NONE', ( #16672 ), #15663, .T. ) ;
#15162 = CARTESIAN_POINT ( 'NONE',  ( 4.499999999999999112, 21.74680007765647360, -0.05647727720537982360 ) ) ;
#15163 = CARTESIAN_POINT ( 'NONE',  ( 8.500000000000001776, 14.99364916731036956, -18.35000000000000142 ) ) ;
#15164 = CARTESIAN_POINT ( 'NONE',  ( 8.499999999999994671, 13.00000000000000178, 22.64999999999999147 ) ) ;
#15165 = CARTESIAN_POINT ( 'NONE',  ( -4.243569643749997233, -19.30147405945127304, -7.555371749410396021 ) ) ;
#15166 = VERTEX_POINT ( 'NONE', #2756 ) ;
#15167 = ADVANCED_FACE ( 'NONE', ( #12651 ), #15980, .F. ) ;
#15168 = CARTESIAN_POINT ( 'NONE',  ( -4.000000000000004441, -28.69037049274104945, -12.66629745740154611 ) ) ;
#15170 = DIRECTION ( 'NONE',  ( -1.000000000000000000, 0.000000000000000000, 3.469446951953612217E-16 ) ) ;
#15169 = STYLED_ITEM ( 'NONE', ( #14363 ), #7836 ) ;
#15171 = CARTESIAN_POINT ( 'NONE',  ( 2.518350579753628971, 39.37180007765647360, 0.7558219633769073242 ) ) ;
#15172 = CARTESIAN_POINT ( 'NONE',  ( -8.000000000000001776, 36.39999999999999147, 2.499999999999998224 ) ) ;
#15173 = CARTESIAN_POINT ( 'NONE',  ( -2.211161402132901799, 35.87180007765648071, -2.942372952327172886 ) ) ;
#15174 = DIRECTION ( 'NONE',  ( -1.000000000000000000, -0.000000000000000000, -0.000000000000000000 ) ) ;
#15175 = CYLINDRICAL_SURFACE ( 'NONE', #6011, 4.000000000000000000 ) ;
#15176 = ORIENTED_EDGE ( 'NONE', *, *, #1744, .F. ) ;
#15177 = VECTOR ( 'NONE', #1684, 1000.000000000000000 ) ;
#15178 = CARTESIAN_POINT ( 'NONE',  ( -2.121784821875005722, -24.02846066063528596, -3.627482962684610346 ) ) ;
#15179 = CARTESIAN_POINT ( 'NONE',  ( 2.115076519116362963, 26.37180007765648071, -3.012182706137107147 ) ) ;
#15180 = AXIS2_PLACEMENT_3D ( 'NONE', #6220, #392, #4832 ) ;
#15181 = ORIENTED_EDGE ( 'NONE', *, *, #10960, .F. ) ;
#15182 = AXIS2_PLACEMENT_3D ( 'NONE', #6073, #7370, #4413 ) ;
#15183 = FACE_OUTER_BOUND ( 'NONE', #17814, .T. ) ;
#15184 = CARTESIAN_POINT ( 'NONE',  ( -4.243569643750004339, -28.69264088791166856, -12.42436771317613875 ) ) ;
#15185 = COLOUR_RGB ( '',0.8941176470588234615, 0.8941176470588234615, 0.8941176470588234615 ) ;
#15186 = CARTESIAN_POINT ( 'NONE',  ( 3.375445829055900404, -25.20600189401019264, -15.83707978931157534 ) ) ;
#15187 = DIRECTION ( 'NONE',  ( 0.000000000000000000, 0.000000000000000000, 1.000000000000000000 ) ) ;
#15188 = EDGE_CURVE ( 'NONE', #12907, #12502, #2351, .T. ) ;
#15189 = FACE_OUTER_BOUND ( 'NONE', #1147, .T. ) ;
#15190 = CARTESIAN_POINT ( 'NONE',  ( 4.243569643749996345, -28.34849502610105176, -11.93287648660273703 ) ) ;
#15191 = ORIENTED_EDGE ( 'NONE', *, *, #137, .F. ) ;
#15192 = DIRECTION ( 'NONE',  ( -0.000000000000000000, -0.000000000000000000, -1.000000000000000000 ) ) ;
#15193 = CIRCLE ( 'NONE', #4821, 0.9999999999999991118 ) ;
#15194 = CARTESIAN_POINT ( 'NONE',  ( 2.000000000000004441, -18.45466017170117112, -8.113982932514955948 ) ) ;
#15195 = CIRCLE ( 'NONE', #2177, 3.799999999999999378 ) ;
#15196 = CARTESIAN_POINT ( 'NONE',  ( -1.135272562821090014, 38.49680007765647360, -3.311245368580554072 ) ) ;
#15197 = EDGE_LOOP ( 'NONE', ( #8801, #9043, #7017, #7344 ) ) ;
#15198 = ORIENTED_EDGE ( 'NONE', *, *, #5747, .F. ) ;
#15199 = CARTESIAN_POINT ( 'NONE',  ( 2.000000000000004441, -23.35873870250257767, -15.11773291118586293 ) ) ;
#15200 =( REPRESENTATION_RELATIONSHIP ('NONE','NONE', #15868, #5199 ) REPRESENTATION_RELATIONSHIP_WITH_TRANSFORMATION ( #5607 )SHAPE_REPRESENTATION_RELATIONSHIP( ) );
#15201 =( NAMED_UNIT ( * ) SI_UNIT ( $, .STERADIAN. ) SOLID_ANGLE_UNIT ( ) );
#15202 = CARTESIAN_POINT ( 'NONE',  ( 1.336863392178569754, 36.25319992234354771, 4.297206761780648421 ) ) ;
#15203 = CARTESIAN_POINT ( 'NONE',  ( -1.999999999999996225, -17.57278640010649795, -6.854536663413863806 ) ) ;
#15204 = CARTESIAN_POINT ( 'NONE',  ( -2.500000000000001332, 24.50319992234354771, -0.05647727720530596601 ) ) ;
#15205 = ORIENTED_EDGE ( 'NONE', *, *, #15672, .T. ) ;
#15206 = CARTESIAN_POINT ( 'NONE',  ( -4.243569643749998122, -23.46348807572352158, -13.49934377078241710 ) ) ;
#15207 = CARTESIAN_POINT ( 'NONE',  ( -4.518350579753632523, 25.62180007765648426, -1.405661355842698468 ) ) ;
#15208 = CARTESIAN_POINT ( 'NONE',  ( 4.000000000000003553, -18.32507965939299055, -5.915763828610126396 ) ) ;
#15209 = ORIENTED_EDGE ( 'NONE', *, *, #10220, .F. ) ;
#15210 = CIRCLE ( 'NONE', #7776, 0.9999999999999991118 ) ;
#15211 = FACE_BOUND ( 'NONE', #1773, .T. ) ;
#15212 = LINE ( 'NONE', #2692, #4120 ) ;
#15213 = FACE_OUTER_BOUND ( 'NONE', #16441, .T. ) ;
#15214 = CARTESIAN_POINT ( 'NONE',  ( 4.730628863548789710E-15, -16.56322023426900714, -7.916230118663721171 ) ) ;
#15215 = CARTESIAN_POINT ( 'NONE',  ( -2.121784821874996396, -19.90043129408965328, -10.54651638600367214 ) ) ;
#15216 = FACE_OUTER_BOUND ( 'NONE', #15467, .T. ) ;
#15217 = ORIENTED_EDGE ( 'NONE', *, *, #3829, .F. ) ;
#15218 = CARTESIAN_POINT ( 'NONE',  ( 1.999999999999994449, -27.05515183642128108, -8.317804239251627152 ) ) ;
#15219 = CARTESIAN_POINT ( 'NONE',  ( -1.661723472263481630E-14, -21.80128239342201724, -13.82776510965112671 ) ) ;
#15220 = TOROIDAL_SURFACE ( 'NONE', #12826, 9.000000000000003553, 0.9999999999999991118 ) ;
#15221 = CARTESIAN_POINT ( 'NONE',  ( 9.000000000000003553, -4.000000000000000000, -30.00000000000000000 ) ) ;
#15222 = ORIENTED_EDGE ( 'NONE', *, *, #6778, .T. ) ;
#15223 = CARTESIAN_POINT ( 'NONE',  ( -1.027846397803611866, 37.50319992234354061, -3.346150245485499219 ) ) ;
#15224 = CARTESIAN_POINT ( 'NONE',  ( 2.864755990943222308, 20.50319992234354416, -2.011557305968548093 ) ) ;
#15225 = CARTESIAN_POINT ( 'NONE',  ( 4.243569643750000786, -19.86730713195397868, -4.091975012412500945 ) ) ;
#15226 = CARTESIAN_POINT ( 'NONE',  ( -2.055738996568313048, 30.74680007765648071, -1.423772053676023441 ) ) ;
#15227 = ADVANCED_FACE ( 'NONE', ( #14949 ), #2243, .T. ) ;
#15228 = CARTESIAN_POINT ( 'NONE',  ( -3.673772985318163098, 24.25319992234354061, 2.599342558261029001 ) ) ;
#15229 = EDGE_CURVE ( 'NONE', #156, #18266, #11801, .T. ) ;
#15230 = CARTESIAN_POINT ( 'NONE',  ( 2.000000000000004441, -21.74555497456032427, -12.81386778561629924 ) ) ;
#15231 = EDGE_LOOP ( 'NONE', ( #12975, #10478, #17404, #3235, #17085 ) ) ;
#15232 = EDGE_CURVE ( 'NONE', #10052, #13486, #7966, .T. ) ;
#15233 = CARTESIAN_POINT ( 'NONE',  ( -5.330712181944245322E-15, -24.49420468597353562, -2.156889308302778030 ) ) ;
#15234 = CARTESIAN_POINT ( 'NONE',  ( 2.211161402132902243, 22.12180007765648071, 2.942372952327172442 ) ) ;
#15235 =( BOUNDED_CURVE ( )  B_SPLINE_CURVE ( 2, ( #6655, #17901, #12302, #6563, #3780, #18264, #16501, #15476, #9522 ),
 .UNSPECIFIED., .F., .F. ) 
 B_SPLINE_CURVE_WITH_KNOTS ( ( 3, 2, 2, 2, 3 ),
 ( 0.4741379310344827624, 0.4770114942528735358, 0.4827586206896551935, 0.4885057471264367956, 0.4913793103448276245 ),
 .UNSPECIFIED. ) 
 CURVE ( )  GEOMETRIC_REPRESENTATION_ITEM ( )  RATIONAL_B_SPLINE_CURVE ( ( 0.9330127018922194093, 0.9330127018922200755, 1.000000000000000000, 0.8660254037844387076, 1.000000000000000000, 0.8660254037844387076, 1.000000000000000000, 0.9330127018922187432, 0.9330127018922194093 ) ) 
 REPRESENTATION_ITEM ( '' )  );
#15236 = FACE_OUTER_BOUND ( 'NONE', #2299, .T. ) ;
#15237 = AXIS2_PLACEMENT_3D ( 'NONE', #7074, #5872, #8463 ) ;
#15238 = EDGE_CURVE ( 'NONE', #7134, #3136, #2062, .T. ) ;
#15239 = CARTESIAN_POINT ( 'NONE',  ( -4.243569643750000786, -24.90044036093436119, -11.28003420104843357 ) ) ;
#15240 = CARTESIAN_POINT ( 'NONE',  ( 1.071796769724490339, -22.84524667957272470, -15.31870062402723320 ) ) ;
#15241 = FACE_OUTER_BOUND ( 'NONE', #17072, .T. ) ;
#15242 = DIRECTION ( 'NONE',  ( 0.000000000000000000, 0.000000000000000000, -1.000000000000000000 ) ) ;
#15243 = EDGE_LOOP ( 'NONE', ( #13256, #776, #13141, #8922 ) ) ;
#15244 = ORIENTED_EDGE ( 'NONE', *, *, #909, .T. ) ;
#15245 = CARTESIAN_POINT ( 'NONE',  ( 0.05938372350927906274, 17.37180007765647005, 3.680117784833935701 ) ) ;
#15246 = EDGE_CURVE ( 'NONE', #5374, #11211, #12401, .T. ) ;
#15247 = LINE ( 'NONE', #15513, #13193 ) ;
#15248 = DIRECTION ( 'NONE',  ( -0.000000000000000000, -0.5735764363510414965, -0.8191520442889950182 ) ) ;
#15249 = CARTESIAN_POINT ( 'NONE',  ( 0.000000000000000000, 5.977523610840987267, 32.81826849749789687 ) ) ;
#15250 = ORIENTED_EDGE ( 'NONE', *, *, #15559, .F. ) ;
#15251 = CARTESIAN_POINT ( 'NONE',  ( -2.518350579753611207, 36.87819992234354061, 0.7558219633769609480 ) ) ;
#15252 = CARTESIAN_POINT ( 'NONE',  ( 4.243569643750003451, -21.96860448848362779, -11.36442875535422026 ) ) ;
#15253 = CARTESIAN_POINT ( 'NONE',  ( -3.518350579753630747, 30.62180007765647716, -1.080741659609802729 ) ) ;
#15254 = PRODUCT_RELATED_PRODUCT_CATEGORY ( 'part', '', ( #6792 ) ) ;
#15255 = CARTESIAN_POINT ( 'NONE',  ( 3.481649420246394122, 23.37819992234353705, 1.193696214020467439 ) ) ;
#15256 = DIRECTION ( 'NONE',  ( -0.000000000000000000, -0.5735764363510414965, -0.8191520442889950182 ) ) ;
#15257 = FACE_OUTER_BOUND ( 'NONE', #5117, .T. ) ;
#15258 = CARTESIAN_POINT ( 'NONE',  ( -4.243569643750005227, -26.40191999523469946, -9.152879236296964649 ) ) ;
#15259 = CARTESIAN_POINT ( 'NONE',  ( 0.000000000000000000, -10.00000000000000178, -12.59063537424807677 ) ) ;
#15260 = CARTESIAN_POINT ( 'NONE',  ( -2.733110507866247652, 22.62180007765647360, 3.862833514489154574 ) ) ;
#15261 = CARTESIAN_POINT ( 'NONE',  ( -1.999999999999996225, -17.89542314625890285, -7.315309689333185261 ) ) ;
#15262 = DIRECTION ( 'NONE',  ( -0.000000000000000000, 1.000000000000000000, -0.000000000000000000 ) ) ;
#15263 = CARTESIAN_POINT ( 'NONE',  ( 4.243569643750000786, -21.67407290645975948, -6.672303951922835097 ) ) ;
#15264 = AXIS2_PLACEMENT_3D ( 'NONE', #7453, #10513, #6598 ) ;
#15265 = DIRECTION ( 'NONE',  ( -0.000000000000000000, -0.5735764363510414965, -0.8191520442889950182 ) ) ;
#15266 = DIRECTION ( 'NONE',  ( -0.000000000000000000, -0.5735764363510414965, -0.8191520442889950182 ) ) ;
#15267 = CARTESIAN_POINT ( 'NONE',  ( 1.989345975306426206, 36.49680007765648071, -1.515154207786343799 ) ) ;
#15268 = CARTESIAN_POINT ( 'NONE',  ( -1.734723475976807094E-15, 31.99999999999999289, -2.500000000000000000 ) ) ;
#15269 = CARTESIAN_POINT ( 'NONE',  ( 2.798362969681366330, 38.99680007765647360, -2.102939460078824929 ) ) ;
#15270 = DIRECTION ( 'NONE',  ( -0.000000000000000000, -1.000000000000000000, -0.000000000000000000 ) ) ;
#15271 = CARTESIAN_POINT ( 'NONE',  ( -3.859945489046901823, 15.00000000000001954, -1.030823890046652869 ) ) ;
#15272 = ORIENTED_EDGE ( 'NONE', *, *, #7679, .F. ) ;
#15273 = CARTESIAN_POINT ( 'NONE',  ( 4.730628863548789710E-15, -17.36981209788766023, -9.068162680945121679 ) ) ;
#15274 = CARTESIAN_POINT ( 'NONE',  ( -2.864755990943265829, 28.24680007765648071, -2.011557305968488141 ) ) ;
#15275 = CARTESIAN_POINT ( 'NONE',  ( -4.243569643750000786, -26.44909673908217584, -13.49174472062871999 ) ) ;
#15276 = AXIS2_PLACEMENT_3D ( 'NONE', #4369, #17015, #15436 ) ;
#15277 = DIRECTION ( 'NONE',  ( -0.000000000000000000, 1.000000000000000000, -0.000000000000000000 ) ) ;
#15278 = LINE ( 'NONE', #6821, #4418 ) ;
#15279 = CARTESIAN_POINT ( 'NONE',  ( -4.000000000000004441, -22.75385437650777476, -4.188073799010446407 ) ) ;
#15280 = CARTESIAN_POINT ( 'NONE',  ( -2.121784821874996396, -23.48169916855646733, -15.66109696253308314 ) ) ;
#15281 = ORIENTED_EDGE ( 'NONE', *, *, #375, .T. ) ;
#15282 = DIRECTION ( 'NONE',  ( 1.000000000000000000, 0.000000000000000000, 0.000000000000000000 ) ) ;
#15283 = CARTESIAN_POINT ( 'NONE',  ( -4.000000000000000888, -21.98057781498731345, -7.110038326093152783 ) ) ;
#15284 = CARTESIAN_POINT ( 'NONE',  ( 3.518350579753631191, 39.37180007765646650, 1.080741659609802285 ) ) ;
#15285 = ORIENTED_EDGE ( 'NONE', *, *, #786, .T. ) ;
#15286 = LINE ( 'NONE', #2586, #1562 ) ;
#15287 = EDGE_CURVE ( 'NONE', #14859, #10059, #12721, .T. ) ;
#15288 = CARTESIAN_POINT ( 'NONE',  ( 1.336863392178569754, 33.75319992234354771, 4.297206761780648421 ) ) ;
#15289 = UNCERTAINTY_MEASURE_WITH_UNIT (LENGTH_MEASURE( 1.000000000000000082E-05 ), #12980, 'distance_accuracy_value', 'NONE');
#15290 = CARTESIAN_POINT ( 'NONE',  ( 9.000000000000000000, 38.59999999999999432, -2.500000000000001332 ) ) ;
#15291 = CARTESIAN_POINT ( 'NONE',  ( -1.497042530366522461, 24.87819992234354771, -2.161531897785030409 ) ) ;
#15292 = VERTEX_POINT ( 'NONE', #9712 ) ;
#15293 = CARTESIAN_POINT ( 'NONE',  ( -2.121784821875005722, -28.41632039872075666, -9.893996101495421414 ) ) ;
#15294 = CARTESIAN_POINT ( 'NONE',  ( -3.673772985318219053, 25.74680007765648426, -2.599342558260952174 ) ) ;
#15295 = ADVANCED_FACE ( 'NONE', ( #15301 ), #5897, .F. ) ;
#15296 = AXIS2_PLACEMENT_3D ( 'NONE', #17213, #130, #12742 ) ;
#15297 = CARTESIAN_POINT ( 'NONE',  ( -2.000000000000005773, -22.90389237762567021, -2.389191317703265316 ) ) ;
#15298 = ORIENTED_EDGE ( 'NONE', *, *, #560, .T. ) ;
#15299 = CARTESIAN_POINT ( 'NONE',  ( 8.399999999999998579, 4.898587196589415787E-16, -4.000000000000001776 ) ) ;
#15300 = LINE ( 'NONE', #8049, #3467 ) ;
#15301 = FACE_OUTER_BOUND ( 'NONE', #12034, .T. ) ;
#15302 = CARTESIAN_POINT ( 'NONE',  ( -2.121784821874996396, -19.64232189773168358, -10.17789796607362618 ) ) ;
#15303 = VERTEX_POINT ( 'NONE', #8143 ) ;
#15304 = CARTESIAN_POINT ( 'NONE',  ( 8.000000000000001776, 38.59999999999999432, -2.500000000000002220 ) ) ;
#15305 = ORIENTED_EDGE ( 'NONE', *, *, #786, .F. ) ;
#15306 = AXIS2_PLACEMENT_3D ( 'NONE', #7934, #12200, #10905 ) ;
#15307 = CARTESIAN_POINT ( 'NONE',  ( -1.999999999999996225, -22.02517348798640029, -13.21320440821394904 ) ) ;
#15308 = CARTESIAN_POINT ( 'NONE',  ( 13.00000000000000178, 15.00000000000000178, 25.00000000000000355 ) ) ;
#15309 = DIRECTION ( 'NONE',  ( 0.000000000000000000, 0.000000000000000000, -1.000000000000000000 ) ) ;
#15310 = CARTESIAN_POINT ( 'NONE',  ( -1.734723475976807094E-15, 43.00000000000000000, -10.50000000000000178 ) ) ;
#15311 = ORIENTED_EDGE ( 'NONE', *, *, #16427, .T. ) ;
#15312 = CARTESIAN_POINT ( 'NONE',  ( 2.798362969681409851, 36.00319992234354771, 2.102939460078764977 ) ) ;
#15313 = CARTESIAN_POINT ( 'NONE',  ( -2.211161402132838738, 21.62819992234354771, 2.942372952327218183 ) ) ;
#15314 = CARTESIAN_POINT ( 'NONE',  ( -4.243569643750005227, -21.98179658260448832, -2.840288794994898058 ) ) ;
#15315 = CARTESIAN_POINT ( 'NONE',  ( -1.497042530366477164, 30.12180007765648426, 2.161531897785062384 ) ) ;
#15316 = EDGE_CURVE ( 'NONE', #8682, #17004, #6505, .T. ) ;
#15317 = CARTESIAN_POINT ( 'NONE',  ( 3.607379964056363075, 28.50319992234354416, 2.690724712371229010 ) ) ;
#15318 = CARTESIAN_POINT ( 'NONE',  ( -4.000000000000000888, -24.23903503241459845, -10.33544949947430425 ) ) ;
#15319 = ORIENTED_EDGE ( 'NONE', *, *, #5115, .T. ) ;
#15320 = CIRCLE ( 'NONE', #7594, 10.00000000000000000 ) ;
#15321 = CARTESIAN_POINT ( 'NONE',  ( -2.864755990943265829, 20.74680007765647716, -2.011557305968488141 ) ) ;
#15322 = CARTESIAN_POINT ( 'NONE',  ( 1.743066579297358403E-15, -23.60804816792780159, -16.40809404916146264 ) ) ;
#15323 = CARTESIAN_POINT ( 'NONE',  ( 4.243569643750003451, -20.67805750669377929, -9.521336655703983354 ) ) ;
#15324 = DIRECTION ( 'NONE',  ( -0.000000000000000000, 1.000000000000000000, -0.000000000000000000 ) ) ;
#15325 = EDGE_CURVE ( 'NONE', #6382, #3333, #13986, .T. ) ;
#15326 = CARTESIAN_POINT ( 'NONE',  ( 14.20000000000000107, 0.000000000000000000, 0.000000000000000000 ) ) ;
#15327 = CARTESIAN_POINT ( 'NONE',  ( -13.00000000000000178, 15.00000000000000178, 25.00000000000000355 ) ) ;
#15328 = ORIENTED_EDGE ( 'NONE', *, *, #4144, .F. ) ;
#15329 = VERTEX_POINT ( 'NONE', #18273 ) ;
#15330 = DIRECTION ( 'NONE',  ( -0.000000000000000000, -1.000000000000000000, -0.000000000000000000 ) ) ;
#15331 = CARTESIAN_POINT ( 'NONE',  ( 9.000000000000001776, 23.19999999999999574, -2.500000000000002665 ) ) ;
#15332 = CARTESIAN_POINT ( 'NONE',  ( -10.00000000000000178, 38.59999999999999432, -2.500000000000001776 ) ) ;
#15333 = FILL_AREA_STYLE_COLOUR ( '', #4976 ) ;
#15334 = VERTEX_POINT ( 'NONE', #12496 ) ;
#15335 = CARTESIAN_POINT ( 'NONE',  ( 0.05938372350921204690, 35.12819992234354771, -2.628655560595669183 ) ) ;
#15336 = AXIS2_PLACEMENT_3D ( 'NONE', #10815, #2579, #6462 ) ;
#15337 = CARTESIAN_POINT ( 'NONE',  ( 2.121784821875004390, -21.71795162677701896, -13.14220442634442243 ) ) ;
#15338 = CARTESIAN_POINT ( 'NONE',  ( 2.864755990943265829, 34.49680007765648071, 2.011557305968487697 ) ) ;
#15339 = CARTESIAN_POINT ( 'NONE',  ( 2.211161402132839626, 27.87819992234354061, -2.942372952327218183 ) ) ;
#15340 = DIRECTION ( 'NONE',  ( 3.469446951953612217E-16, -0.000000000000000000, 1.000000000000000000 ) ) ;
#15341 = DIRECTION ( 'NONE',  ( -1.000000000000000000, 0.000000000000000000, 4.336808689942021680E-16 ) ) ;
#15342 = CARTESIAN_POINT ( 'NONE',  ( -4.243569643750005227, -25.62759180616079746, -8.047023976506819665 ) ) ;
#15343 = CLOSED_SHELL ( 'NONE', ( #14869, #7732, #9879, #3759, #9665, #13049, #2262, #13848, #5112, #10282 ) ) ;
#15344 = CIRCLE ( 'NONE', #1720, 0.1999999999999987899 ) ;
#15345 = AXIS2_PLACEMENT_3D ( 'NONE', #13394, #12361, #6530 ) ;
#15346 = CYLINDRICAL_SURFACE ( 'NONE', #1407, 0.9999999999999991118 ) ;
#15347 = EDGE_CURVE ( 'NONE', #456, #14275, #14805, .T. ) ;
#15348 = ADVANCED_FACE ( 'NONE', ( #9892 ), #7110, .T. ) ;
#15349 = DIRECTION ( 'NONE',  ( -1.000000000000000000, 0.000000000000000000, 4.336808689942021680E-16 ) ) ;
#15350 = EDGE_CURVE ( 'NONE', #4080, #7871, #11194, .T. ) ;
#15351 = DIRECTION ( 'NONE',  ( -0.000000000000000000, 1.000000000000000000, -0.000000000000000000 ) ) ;
#15352 = CARTESIAN_POINT ( 'NONE',  ( 4.243569643750003451, -20.16183871397784344, -8.784099815843886105 ) ) ;
#15353 = CARTESIAN_POINT ( 'NONE',  ( 1.743066579297358403E-15, -23.60804816792780159, -16.40809404916146264 ) ) ;
#15354 = FILL_AREA_STYLE ('',( #3003 ) ) ;
#15355 = CARTESIAN_POINT ( 'NONE',  ( 1.593127413382998903, 39.62180007765647360, 2.091722143975139669 ) ) ;
#15356 = CIRCLE ( 'NONE', #16537, 2.149999999999995470 ) ;
#15357 = DIRECTION ( 'NONE',  ( -3.373073425510457965E-16, 0.000000000000000000, -1.000000000000000000 ) ) ;
#15358 = CARTESIAN_POINT ( 'NONE',  ( -2.115076519116362519, 37.62180007765647360, 3.012182706137108035 ) ) ;
#15359 = CARTESIAN_POINT ( 'NONE',  ( -1.071796769724486564, -28.49508014663179623, -9.439924663463729715 ) ) ;
#15360 = CONTEXT_DEPENDENT_SHAPE_REPRESENTATION ( #8893, #13902 ) ;
#15361 = PRESENTATION_LAYER_ASSIGNMENT (  '', '', ( #17434 ) ) ;
#15362 = CARTESIAN_POINT ( 'NONE',  ( -3.721472675004220854, 15.00000000000001421, -1.423657464930958128 ) ) ;
#15363 = AXIS2_PLACEMENT_3D ( 'NONE', #1051, #12065, #10680 ) ;
#15364 = EDGE_LOOP ( 'NONE', ( #15847, #6092 ) ) ;
#15365 = CARTESIAN_POINT ( 'NONE',  ( -2.121784821875005722, -24.80278884970919506, -4.733338222474753998 ) ) ;
#15366 = CARTESIAN_POINT ( 'NONE',  ( 2.115076519116362963, 21.37180007765648071, -3.012182706137107147 ) ) ;
#15367 = FACE_OUTER_BOUND ( 'NONE', #8152, .T. ) ;
#15368 = CARTESIAN_POINT ( 'NONE',  ( -2.121784821874996396, -23.48169916855646733, -15.66109696253308314 ) ) ;
#15369 = CARTESIAN_POINT ( 'NONE',  ( -5.577813053751546416E-15, -24.87002189690140241, -4.262804949787145858 ) ) ;
#15370 = AXIS2_PLACEMENT_3D ( 'NONE', #9472, #15330, #6689 ) ;
#15371 = DIRECTION ( 'NONE',  ( 0.000000000000000000, 1.000000000000000000, 0.000000000000000000 ) ) ;
#15372 = AXIS2_PLACEMENT_3D ( 'NONE', #15865, #188, #5837 ) ;
#15373 = CARTESIAN_POINT ( 'NONE',  ( 4.243569643749996345, -27.57416683702714622, -10.82702122681259205 ) ) ;
#15374 = VERTEX_POINT ( 'NONE', #2783 ) ;
#15375 = FACE_OUTER_BOUND ( 'NONE', #6984, .T. ) ;
#15376 = CARTESIAN_POINT ( 'NONE',  ( 3.999999999999996447, -23.50667344992347196, -5.263210858146513793 ) ) ;
#15377 = CARTESIAN_POINT ( 'NONE',  ( -1.135272562821090014, 35.99680007765648071, -3.311245368580554072 ) ) ;
#15378 = ORIENTED_EDGE ( 'NONE', *, *, #31, .T. ) ;
#15379 = CARTESIAN_POINT ( 'NONE',  ( -2.343145750507622527, 4.000000000000006217, 3.999999999999999112 ) ) ;
#15380 = EDGE_CURVE ( 'NONE', #16617, #11774, #12771, .T. ) ;
#15381 =( NAMED_UNIT ( * ) PLANE_ANGLE_UNIT ( ) SI_UNIT ( $, .RADIAN. ) );
#15382 = CARTESIAN_POINT ( 'NONE',  ( 4.499999999999999112, 16.74680007765647716, -0.05647727720537982360 ) ) ;
#15383 = VECTOR ( 'NONE', #17609, 1000.000000000000000 ) ;
#15384 = CARTESIAN_POINT ( 'NONE',  ( 8.000000000000000000, 46.00000000000000000, 2.500000000000000000 ) ) ;
#15385 = CARTESIAN_POINT ( 'NONE',  ( 2.500000000000001332, 28.25319992234354771, 0.05647727720530566764 ) ) ;
#15386 = ORIENTED_EDGE ( 'NONE', *, *, #7906, .F. ) ;
#15387 = CARTESIAN_POINT ( 'NONE',  ( -4.243569643750000786, -25.19081343183707844, -11.69472992346973861 ) ) ;
#15388 = CARTESIAN_POINT ( 'NONE',  ( -4.481649420246366589, 22.87180007765647360, 1.518615910253458878 ) ) ;
#15389 = CARTESIAN_POINT ( 'NONE',  ( -3.999999999999997335, -17.98093379758235955, -5.424272602036731783 ) ) ;
#15390 = ORIENTED_EDGE ( 'NONE', *, *, #6928, .T. ) ;
#15391 = FACE_OUTER_BOUND ( 'NONE', #1643, .T. ) ;
#15392 = EDGE_CURVE ( 'NONE', #723, #3667, #15680, .T. ) ;
#15393 = CARTESIAN_POINT ( 'NONE',  ( -2.000000000000005773, -26.84006067278963670, -8.010622222643258183 ) ) ;
#15394 = CARTESIAN_POINT ( 'NONE',  ( -8.500000000000007105, 14.99364916731036956, -20.49999999999999645 ) ) ;
#15395 = CARTESIAN_POINT ( 'NONE',  ( -8.500000000000005329, 0.000000000000000000, 20.49999999999999645 ) ) ;
#15396 = VECTOR ( 'NONE', #13572, 1000.000000000000000 ) ;
#15397 = CARTESIAN_POINT ( 'NONE',  ( 4.730628863548789710E-15, -19.43468726875141073, -12.01711004038550001 ) ) ;
#15398 = ADVANCED_FACE ( 'NONE', ( #5458 ), #1386, .T. ) ;
#15399 = ORIENTED_EDGE ( 'NONE', *, *, #14899, .F. ) ;
#15400 = AXIS2_PLACEMENT_3D ( 'NONE', #15544, #8210, #13874 ) ;
#15401 = CARTESIAN_POINT ( 'NONE',  ( 3.579096709490575479E-14, -26.48320562484364871, -6.566670075356708658 ) ) ;
#15402 = EDGE_CURVE ( 'NONE', #4416, #8124, #3549, .T. ) ;
#15403 = ORIENTED_EDGE ( 'NONE', *, *, #6483, .F. ) ;
#15404 = CARTESIAN_POINT ( 'NONE',  ( 4.000000000000000888, -24.94883587310395967, -11.34915015528869731 ) ) ;
#15405 = CARTESIAN_POINT ( 'NONE',  ( 0.000000000000000000, 5.977523610840987267, 32.81826849749789687 ) ) ;
#15406 = CARTESIAN_POINT ( 'NONE',  ( 0.05938372350927906967, 22.37180007765648071, 3.680117784833935701 ) ) ;
#15407 = CARTESIAN_POINT ( 'NONE',  ( 0.000000000000000000, 10.00000000000000000, 0.000000000000000000 ) ) ;
#15408 = ORIENTED_EDGE ( 'NONE', *, *, #10323, .T. ) ;
#15409 = CARTESIAN_POINT ( 'NONE',  ( 3.607379964056363075, 16.00319992234354416, 2.690724712371229010 ) ) ;
#15410 = CARTESIAN_POINT ( 'NONE',  ( -2.864755990943222308, 21.75319992234354771, 2.011557305968548093 ) ) ;
#15411 = CARTESIAN_POINT ( 'NONE',  ( 3.999999999999996447, -27.37831439529299615, -10.79248715709723072 ) ) ;
#15412 = CARTESIAN_POINT ( 'NONE',  ( 2.518350579753628971, 29.37180007765648426, 0.7558219633769073242 ) ) ;
#15413 = CARTESIAN_POINT ( 'NONE',  ( 3.673772985318163098, 23.00319992234354416, -2.599342558261029001 ) ) ;
#15414 = CARTESIAN_POINT ( 'NONE',  ( -1.999999999999996225, -22.47686493090789739, -13.85828664208477079 ) ) ;
#15415 = ORIENTED_EDGE ( 'NONE', *, *, #3090, .T. ) ;
#15416 = AXIS2_PLACEMENT_3D ( 'NONE', #18165, #5435, #3115 ) ;
#15417 = CARTESIAN_POINT ( 'NONE',  ( -4.243569643750005227, -22.01406025714923231, -2.886366097486154469 ) ) ;
#15418 = CARTESIAN_POINT ( 'NONE',  ( -2.864755990943265829, 18.24680007765648071, -2.011557305968488141 ) ) ;
#15419 = SURFACE_STYLE_USAGE ( .BOTH. , #5390 ) ;
#15420 = CARTESIAN_POINT ( 'NONE',  ( -4.243569643750000786, -23.35178398278655010, -9.068323681468148934 ) ) ;
#15421 = DIRECTION ( 'NONE',  ( 0.000000000000000000, 1.000000000000000000, 0.000000000000000000 ) ) ;
#15422 = DIRECTION ( 'NONE',  ( 0.000000000000000000, 0.000000000000000000, 1.000000000000000000 ) ) ;
#15423 = CARTESIAN_POINT ( 'NONE',  ( -8.500000000000005329, 15.00000000000000178, -22.64999999999999147 ) ) ;
#15424 = EDGE_CURVE ( 'NONE', #5921, #2131, #8549, .T. ) ;
#15425 = ORIENTED_EDGE ( 'NONE', *, *, #1321, .T. ) ;
#15426 = EDGE_LOOP ( 'NONE', ( #6840, #962, #17856, #16956 ) ) ;
#15427 = CARTESIAN_POINT ( 'NONE',  ( -1.135272562821090014, 23.49680007765647716, -3.311245368580554072 ) ) ;
#15428 = DIRECTION ( 'NONE',  ( -0.000000000000000000, -1.000000000000000000, -0.000000000000000000 ) ) ;
#15429 = CARTESIAN_POINT ( 'NONE',  ( 0.000000000000000000, 23.19999999999999574, 2.500000000000000000 ) ) ;
#15430 = ORIENTED_EDGE ( 'NONE', *, *, #16232, .F. ) ;
#15431 = VECTOR ( 'NONE', #3462, 1000.000000000000000 ) ;
#15432 = CARTESIAN_POINT ( 'NONE',  ( 1.497042530366522461, 38.62819992234354771, 2.161531897785029965 ) ) ;
#15433 = CARTESIAN_POINT ( 'NONE',  ( -4.243569643750000786, -23.35178398278655010, -9.068323681468148934 ) ) ;
#15434 = CARTESIAN_POINT ( 'NONE',  ( -3.481649420246369697, 27.87180007765647360, 1.193696214020542490 ) ) ;
#15435 = CARTESIAN_POINT ( 'NONE',  ( 2.864755990943222308, 30.50319992234354416, -2.011557305968548093 ) ) ;
#15436 = DIRECTION ( 'NONE',  ( 0.000000000000000000, 0.000000000000000000, -1.000000000000000000 ) ) ;
#15437 = CYLINDRICAL_SURFACE ( 'NONE', #12304, 0.9999999999999991118 ) ;
#15438 = B_SPLINE_CURVE_WITH_KNOTS ( 'NONE', 3,
 ( #16184, #7911, #3480, #3661, #9393, #13566, #9126, #4952 ),
 .UNSPECIFIED., .F., .F.,
 ( 4, 2, 2, 4 ),
 ( 0.02025600316476611554, 0.02089043502514349032, 0.02152486688552086164, 0.02279373060627560774 ),
 .UNSPECIFIED. ) ;
#15439 = CARTESIAN_POINT ( 'NONE',  ( -4.243569643750000786, -23.38404765733129764, -9.114400983959404456 ) ) ;
#15440 = CIRCLE ( 'NONE', #2987, 0.9999999999999991118 ) ;
#15441 = CARTESIAN_POINT ( 'NONE',  ( -9.000000000000001776, 38.59999999999999432, 2.499999999999995559 ) ) ;
#15442 = DIRECTION ( 'NONE',  ( 0.000000000000000000, 0.000000000000000000, 1.000000000000000000 ) ) ;
#15443 = CARTESIAN_POINT ( 'NONE',  ( 4.299564228933482956E-15, -17.73605940148895854, -8.022024996759636650 ) ) ;
#15444 = CARTESIAN_POINT ( 'NONE',  ( 4.730628863548789710E-15, -18.36998600877478438, -10.49655905817405355 ) ) ;
#15445 = FACE_BOUND ( 'NONE', #1142, .T. ) ;
#15446 = DIRECTION ( 'NONE',  ( -1.000000000000000000, 0.000000000000000000, 0.000000000000000000 ) ) ;
#15447 = CARTESIAN_POINT ( 'NONE',  ( 0.7188294034286553114, 16.25319992234354771, 2.395093729190349130 ) ) ;
#15448 = CYLINDRICAL_SURFACE ( 'NONE', #12382, 4.000000000000000000 ) ;
#15449 = CARTESIAN_POINT ( 'NONE',  ( 0.000000000000000000, 33.00000000000000000, 0.000000000000000000 ) ) ;
#15450 = CARTESIAN_POINT ( 'NONE',  ( 0.000000000000000000, 0.000000000000000000, 0.000000000000000000 ) ) ;
#15451 = VECTOR ( 'NONE', #10203, 1000.000000000000000 ) ;
#15452 = CARTESIAN_POINT ( 'NONE',  ( -8.999999999999996447, -4.000000000000000000, 30.00000000000000000 ) ) ;
#15453 = EDGE_CURVE ( 'NONE', #1682, #17585, #18068, .T. ) ;
#15454 = ORIENTED_EDGE ( 'NONE', *, *, #12603, .F. ) ;
#15455 = CARTESIAN_POINT ( 'NONE',  ( -2.121784821874996396, -18.86799370865777803, -9.072042706283481195 ) ) ;
#15456 = CARTESIAN_POINT ( 'NONE',  ( -3.500000000000000444, 32.99680007765648071, 0.05647727720536892260 ) ) ;
#15457 = EDGE_CURVE ( 'NONE', #3719, #17766, #2946, .T. ) ;
#15458 = EDGE_CURVE ( 'NONE', #13335, #8355, #10344, .T. ) ;
#15459 = DIRECTION ( 'NONE',  ( -0.000000000000000000, -1.000000000000000000, -0.000000000000000000 ) ) ;
#15460 = CARTESIAN_POINT ( 'NONE',  ( -4.243569643749998122, -24.97988077932658157, -15.66497698787144799 ) ) ;
#15461 = DIRECTION ( 'NONE',  ( -0.000000000000000000, -0.000000000000000000, -1.000000000000000000 ) ) ;
#15462 = EDGE_CURVE ( 'NONE', #6724, #4967, #15105, .T. ) ;
#15463 = CARTESIAN_POINT ( 'NONE',  ( -5.577813053751546416E-15, -25.64435008597530796, -5.368660209577289955 ) ) ;
#15464 = TOROIDAL_SURFACE ( 'NONE', #4485, 9.000000000000001776, 0.9999999999999991118 ) ;
#15465 = CARTESIAN_POINT ( 'NONE',  ( -5.577813053751546416E-15, -29.32240898478130120, -10.62147269458723464 ) ) ;
#15466 = CARTESIAN_POINT ( 'NONE',  ( 4.730628863548789710E-15, -22.75784574686025152, -16.76307219698486506 ) ) ;
#15467 = EDGE_LOOP ( 'NONE', ( #6003, #6262, #746, #9203 ) ) ;
#15468 = CARTESIAN_POINT ( 'NONE',  ( -1.999999999999996225, -20.67009915640211659, -11.27795770257443841 ) ) ;
#15469 = CARTESIAN_POINT ( 'NONE',  ( -2.000000000000005773, -24.25896670920994680, -4.324438023342780824 ) ) ;
#15470 = CARTESIAN_POINT ( 'NONE',  ( 2.055738996568313048, 16.99680007765648071, 1.423772053676023441 ) ) ;
#15471 = ORIENTED_EDGE ( 'NONE', *, *, #14075, .T. ) ;
#15472 = DIRECTION ( 'NONE',  ( 0.000000000000000000, 0.8191520442889952403, -0.5735764363510413855 ) ) ;
#15473 = VECTOR ( 'NONE', #5959, 1000.000000000000000 ) ;
#15474 = CARTESIAN_POINT ( 'NONE',  ( 4.499999999999999112, 38.25319992234354061, 0.05647727720528474687 ) ) ;
#15475 = CIRCLE ( 'NONE', #969, 0.9999999999999991118 ) ;
#15476 = CARTESIAN_POINT ( 'NONE',  ( 1.071796769724485454, -20.26415271599303836, -11.63251642472675229 ) ) ;
#15477 = CARTESIAN_POINT ( 'NONE',  ( 1.497042530366522461, 36.12819992234354771, 2.161531897785029965 ) ) ;
#15478 = ORIENTED_EDGE ( 'NONE', *, *, #18139, .F. ) ;
#15479 = CARTESIAN_POINT ( 'NONE',  ( -2.121784821875005722, -27.90010160600482081, -9.156759261635325942 ) ) ;
#15480 = AXIS2_PLACEMENT_3D ( 'NONE', #2492, #15371, #1360 ) ;
#15481 = CARTESIAN_POINT ( 'NONE',  ( 4.499999999999999112, 36.74680007765647360, -0.05647727720537982360 ) ) ;
#15482 = ORIENTED_EDGE ( 'NONE', *, *, #1230, .T. ) ;
#15483 = FILL_AREA_STYLE_COLOUR ( '', #18088 ) ;
#15484 = DIRECTION ( 'NONE',  ( 0.000000000000000000, 0.000000000000000000, 1.000000000000000000 ) ) ;
#15485 = AXIS2_PLACEMENT_3D ( 'NONE', #270, #11377, #4435 ) ;
#15486 = DIRECTION ( 'NONE',  ( 0.000000000000000000, 1.000000000000000000, 0.000000000000000000 ) ) ;
#15487 = CARTESIAN_POINT ( 'NONE',  ( -2.121784821874996396, -19.12610310501574418, -9.440661126213528931 ) ) ;
#15488 = ORIENTED_EDGE ( 'NONE', *, *, #14795, .T. ) ;
#15489 = DIRECTION ( 'NONE',  ( -0.000000000000000000, 1.000000000000000000, -0.000000000000000000 ) ) ;
#15490 = VERTEX_POINT ( 'NONE', #13138 ) ;
#15491 = CARTESIAN_POINT ( 'NONE',  ( -3.999999999999997335, -22.43332088546226188, -11.78294034683682057 ) ) ;
#15492 = DIRECTION ( 'NONE',  ( -0.000000000000000000, -1.000000000000000000, -0.000000000000000000 ) ) ;
#15493 = DIRECTION ( 'NONE',  ( 0.000000000000000000, 0.000000000000000000, 1.000000000000000000 ) ) ;
#15494 = CARTESIAN_POINT ( 'NONE',  ( -4.481649420246396787, 19.62819992234354416, -1.518615910253363399 ) ) ;
#15495 = CARTESIAN_POINT ( 'NONE',  ( 0.05938372350920110426, 22.62819992234354416, -3.680117784833935701 ) ) ;
#15496 = CARTESIAN_POINT ( 'NONE',  ( 1.999999999999994449, -29.63624580000097097, -12.00398843855210629 ) ) ;
#15497 = CARTESIAN_POINT ( 'NONE',  ( 2.055738996568313048, 36.99680007765647360, 1.423772053676023441 ) ) ;
#15498 = AXIS2_PLACEMENT_3D ( 'NONE', #8905, #1887, #14682 ) ;
#15499 = CARTESIAN_POINT ( 'NONE',  ( -3.673772985318163098, 26.75319992234354771, 2.599342558261029001 ) ) ;
#15500 = AXIS2_PLACEMENT_3D ( 'NONE', #9002, #11964, #14677 ) ;
#15501 = CARTESIAN_POINT ( 'NONE',  ( 3.999999999999996447, -25.24891187463481046, -7.751385191667569785 ) ) ;
#15502 =( BOUNDED_CURVE ( )  B_SPLINE_CURVE ( 2, ( #10120, #14698, #17491, #7439, #17394, #14508, #217, #10503, #4660 ),
 .UNSPECIFIED., .F., .T. ) 
 B_SPLINE_CURVE_WITH_KNOTS ( ( 3, 2, 2, 2, 3 ),
 ( 0.8534482758620689502, 0.8563218390804597790, 0.8620689655172413257, 0.8678160919540229834, 0.8706896551724138122 ),
 .UNSPECIFIED. ) 
 CURVE ( )  GEOMETRIC_REPRESENTATION_ITEM ( )  RATIONAL_B_SPLINE_CURVE ( ( 0.9330127018922194093, 0.9330127018922194093, 1.000000000000000000, 0.8660254037844387076, 1.000000000000000000, 0.8660254037844387076, 1.000000000000000000, 0.9330127018922194093, 0.9330127018922194093 ) ) 
 REPRESENTATION_ITEM ( '' )  );
#15503 = ORIENTED_EDGE ( 'NONE', *, *, #6349, .F. ) ;
#15504 = CARTESIAN_POINT ( 'NONE',  ( -10.00000000000000178, 43.00000000000000000, -2.500000000000001776 ) ) ;
#15505 = CARTESIAN_POINT ( 'NONE',  ( -0.05938372350927861171, 23.62180007765647005, -3.680117784833935701 ) ) ;
#15506 = CARTESIAN_POINT ( 'NONE',  ( -2.121784821874996396, -19.86816761954490573, -10.50043908351241662 ) ) ;
#15507 = DIRECTION ( 'NONE',  ( 0.8191520442889960174, 0.4698463103929512164, -0.3289899283371594541 ) ) ;
#15508 = CARTESIAN_POINT ( 'NONE',  ( 4.000000000000000888, -21.01266757793999318, -5.727719250348704882 ) ) ;
#15509 = CARTESIAN_POINT ( 'NONE',  ( -1.734723475976807094E-15, 34.19999999999999574, -2.500000000000000000 ) ) ;
#15510 = ORIENTED_EDGE ( 'NONE', *, *, #16558, .F. ) ;
#15511 = EDGE_LOOP ( 'NONE', ( #2852, #13909, #13421, #11557 ) ) ;
#15512 = CARTESIAN_POINT ( 'NONE',  ( 1.135272562821090458, 22.24680007765648071, 3.311245368580554072 ) ) ;
#15513 = CARTESIAN_POINT ( 'NONE',  ( 4.898587196589413815E-16, 2.700915433685006750, 35.11257424290206330 ) ) ;
#15514 = DIRECTION ( 'NONE',  ( -3.469446951953613696E-16, -0.000000000000000000, -1.000000000000000000 ) ) ;
#15515 = DIRECTION ( 'NONE',  ( -0.000000000000000000, 1.000000000000000000, -0.000000000000000000 ) ) ;
#15516 = ORIENTED_EDGE ( 'NONE', *, *, #10205, .T. ) ;
#15517 = CARTESIAN_POINT ( 'NONE',  ( -2.864755990943222308, 21.75319992234354771, 2.011557305968548093 ) ) ;
#15518 = CARTESIAN_POINT ( 'NONE',  ( 4.243569643750003451, -20.41994811033581314, -9.152718235773933841 ) ) ;
#15519 = CARTESIAN_POINT ( 'NONE',  ( -2.115076519116362519, 40.12180007765648071, 3.012182706137107147 ) ) ;
#15520 = CARTESIAN_POINT ( 'NONE',  ( -3.500000000000000444, 27.00319992234354771, -0.05647727720529563400 ) ) ;
#15521 = LINE ( 'NONE', #11406, #10219 ) ;
#15522 = CARTESIAN_POINT ( 'NONE',  ( 0.000000000000000000, -15.45745613286697839, -10.86990606519494129 ) ) ;
#15523 = AXIS2_PLACEMENT_3D ( 'NONE', #8000, #6619, #13655 ) ;
#15524 = CARTESIAN_POINT ( 'NONE',  ( -4.243569643750000786, -23.64215705368926379, -9.483019403889452192 ) ) ;
#15525 = EDGE_CURVE ( 'NONE', #7134, #17274, #286, .T. ) ;
#15526 = CARTESIAN_POINT ( 'NONE',  ( -1.598251304517731564, -15.40332308709088061, -10.50456014341368416 ) ) ;
#15527 = DIRECTION ( 'NONE',  ( -1.000000000000000000, 0.000000000000000000, 4.336808689942021680E-16 ) ) ;
#15528 = CARTESIAN_POINT ( 'NONE',  ( -1.071796769724496334, -24.17174775834076073, -3.265566130642198139 ) ) ;
#15529 = CARTESIAN_POINT ( 'NONE',  ( 4.243569643750000786, -20.38352592466991808, -4.829211852272596417 ) ) ;
#15530 = DIRECTION ( 'NONE',  ( -1.000000000000000000, 0.000000000000000000, 4.336808689942021680E-16 ) ) ;
#15531 = LINE ( 'NONE', #8638, #4965 ) ;
#15532 = ORIENTED_EDGE ( 'NONE', *, *, #2242, .T. ) ;
#15533 = CARTESIAN_POINT ( 'NONE',  ( -0.7188294034286550893, 17.50319992234354771, -2.395093729190349130 ) ) ;
#15534 = DIRECTION ( 'NONE',  ( 0.000000000000000000, 0.000000000000000000, 1.000000000000000000 ) ) ;
#15535 = DIRECTION ( 'NONE',  ( -0.000000000000000000, -0.5735764363510414965, -0.8191520442889950182 ) ) ;
#15536 = CARTESIAN_POINT ( 'NONE',  ( -8.000000000000001776, 23.19999999999999574, 2.499999999999995115 ) ) ;
#15537 = EDGE_LOOP ( 'NONE', ( #6148, #7989, #8428, #3794 ) ) ;
#15538 = CARTESIAN_POINT ( 'NONE',  ( 4.730628863548789710E-15, -16.59548390881375468, -7.962307421154977582 ) ) ;
#15539 = CARTESIAN_POINT ( 'NONE',  ( -2.211161402132902243, 35.87180007765648782, -2.942372952327172886 ) ) ;
#15540 =( REPRESENTATION_RELATIONSHIP ('NONE','NONE', #15868, #12769 ) REPRESENTATION_RELATIONSHIP_WITH_TRANSFORMATION ( #5147 )SHAPE_REPRESENTATION_RELATIONSHIP( ) );
#15541 = DIRECTION ( 'NONE',  ( -0.000000000000000000, -0.000000000000000000, 1.000000000000000000 ) ) ;
#15542 = CARTESIAN_POINT ( 'NONE',  ( 4.243569643749997233, -27.83227623338511236, -11.19563964674263978 ) ) ;
#15543 = CARTESIAN_POINT ( 'NONE',  ( 9.000000000000001776, 38.59999999999999432, -2.500000000000002665 ) ) ;
#15544 = CARTESIAN_POINT ( 'NONE',  ( -9.000000000000001776, 23.19999999999999574, 2.499999999999995559 ) ) ;
#15545 = DIRECTION ( 'NONE',  ( -0.000000000000000000, 1.000000000000000000, -0.000000000000000000 ) ) ;
#15546 = CARTESIAN_POINT ( 'NONE',  ( 4.243569643749996345, -26.54172925159527452, -9.352547547092401103 ) ) ;
#15547 = EDGE_CURVE ( 'NONE', #451, #11984, #4604, .T. ) ;
#15548 = ORIENTED_EDGE ( 'NONE', *, *, #5873, .F. ) ;
#15549 = DIRECTION ( 'NONE',  ( 0.000000000000000000, 0.000000000000000000, 1.000000000000000000 ) ) ;
#15550 = CARTESIAN_POINT ( 'NONE',  ( 4.000000000000000888, -19.78664794594458698, -3.976781756687743918 ) ) ;
#15551 = CARTESIAN_POINT ( 'NONE',  ( -2.481649420246374138, 17.87180007765647716, 0.8687765177876256573 ) ) ;
#15552 = EDGE_CURVE ( 'NONE', #7377, #2690, #1754, .T. ) ;
#15553 = ORIENTED_EDGE ( 'NONE', *, *, #10792, .T. ) ;
#15554 = CARTESIAN_POINT ( 'NONE',  ( -1.661723472263481630E-14, -20.57526276142661459, -12.07682761599016175 ) ) ;
#15555 = CARTESIAN_POINT ( 'NONE',  ( 2.000000000000004441, -20.45500799277048287, -10.97077568596606056 ) ) ;
#15556 = CARTESIAN_POINT ( 'NONE',  ( 1.593127413382953383, 32.87819992234354771, -2.091722143975172532 ) ) ;
#15557 = ORIENTED_EDGE ( 'NONE', *, *, #6159, .F. ) ;
#15558 = CARTESIAN_POINT ( 'NONE',  ( 4.730628863548789710E-15, -20.72523425054125212, -13.86020214003574047 ) ) ;
#15559 = EDGE_CURVE ( 'NONE', #1143, #6012, #17479, .T. ) ;
#15560 = CARTESIAN_POINT ( 'NONE',  ( 3.673772985318219053, 31.99680007765648071, 2.599342558260951730 ) ) ;
#15561 = EDGE_LOOP ( 'NONE', ( #17142, #13346, #11308, #6269 ) ) ;
#15562 = CYLINDRICAL_SURFACE ( 'NONE', #4620, 2.000000000000001776 ) ;
#15563 = CARTESIAN_POINT ( 'NONE',  ( 1.300000000000000044, 0.000000000000000000, 0.000000000000000000 ) ) ;
#15564 = CARTESIAN_POINT ( 'NONE',  ( -4.243569643749997233, -20.62428471578586553, -9.444541151551892000 ) ) ;
#15565 = VERTEX_POINT ( 'NONE', #7382 ) ;
#15566 = DIRECTION ( 'NONE',  ( -0.000000000000000000, -1.000000000000000000, -0.000000000000000000 ) ) ;
#15567 = ADVANCED_FACE ( 'NONE', ( #12949 ), #6188, .T. ) ;
#15568 = VERTEX_POINT ( 'NONE', #5815 ) ;
#15569 = CARTESIAN_POINT ( 'NONE',  ( 2.000000000000004441, -21.55197292799679687, -12.53740397167552878 ) ) ;
#15570 = VECTOR ( 'NONE', #11407, 1000.000000000000000 ) ;
#15571 = FACE_BOUND ( 'NONE', #11665, .T. ) ;
#15572 = DIRECTION ( 'NONE',  ( 0.000000000000000000, 1.000000000000000000, 0.000000000000000000 ) ) ;
#15573 = CARTESIAN_POINT ( 'NONE',  ( 4.499999999999999112, 20.75319992234354416, 0.05647727720528474687 ) ) ;
#15574 = CARTESIAN_POINT ( 'NONE',  ( -3.518350579753606322, 26.87819992234354771, 1.080741659609877781 ) ) ;
#15575 = CARTESIAN_POINT ( 'NONE',  ( -5.279047395330986450E-15, -30.08741143020316144, -10.63516078049664948 ) ) ;
#15576 = AXIS2_PLACEMENT_3D ( 'NONE', #10318, #14410, #15999 ) ;
#15577 = CARTESIAN_POINT ( 'NONE',  ( 1.593127413382953383, 15.37819992234354594, -2.091722143975172532 ) ) ;
#15578 = CARTESIAN_POINT ( 'NONE',  ( 3.607379964056363075, 33.50319992234354061, 2.690724712371229010 ) ) ;
#15579 = CARTESIAN_POINT ( 'NONE',  ( 4.713407268011036227E-15, -20.26195175892625855, -12.70822176395157044 ) ) ;
#15580 = ORIENTED_EDGE ( 'NONE', *, *, #11307, .F. ) ;
#15581 = DIRECTION ( 'NONE',  ( 0.000000000000000000, 0.000000000000000000, 1.000000000000000000 ) ) ;
#15582 = CARTESIAN_POINT ( 'NONE',  ( 2.115076519116362963, 21.37180007765648071, -3.012182706137107147 ) ) ;
#15583 = CARTESIAN_POINT ( 'NONE',  ( -6.428571428571427937, -11.73421655796351892, 14.25837509840160067 ) ) ;
#15584 = CARTESIAN_POINT ( 'NONE',  ( -5.330712181944246111E-15, -27.04303497500847797, -5.796996205112000311 ) ) ;
#15585 = ADVANCED_FACE ( 'NONE', ( #7288 ), #259, .F. ) ;
#15586 = CONICAL_SURFACE ( 'NONE', #794, 2.000000000000001776, 1.029744260000000189 ) ;
#15587 = CARTESIAN_POINT ( 'NONE',  ( 2.733110507866247652, 26.37180007765647716, -3.862833514489153686 ) ) ;
#15588 = CARTESIAN_POINT ( 'NONE',  ( -1.071796769724496334, -20.30562666434980912, -11.69174736140419135 ) ) ;
#15589 = DIRECTION ( 'NONE',  ( 3.469446951953612217E-16, -0.000000000000000000, 1.000000000000000000 ) ) ;
#15590 = ORIENTED_EDGE ( 'NONE', *, *, #15458, .T. ) ;
#15591 = EDGE_LOOP ( 'NONE', ( #352, #16266, #13809, #7142, #4230 ) ) ;
#15592 = CARTESIAN_POINT ( 'NONE',  ( 2.115076519116362963, 21.37180007765648071, -3.012182706137107147 ) ) ;
#15593 = CARTESIAN_POINT ( 'NONE',  ( -1.734723475976807094E-15, 23.19999999999999574, -2.500000000000000000 ) ) ;
#15594 = CARTESIAN_POINT ( 'NONE',  ( -8.500000000000007105, 15.00000000000000000, -18.29999999999999716 ) ) ;
#15595 = CARTESIAN_POINT ( 'NONE',  ( -8.500000000000005329, 13.00000000000000000, -20.49999999999999645 ) ) ;
#15596 = ORIENTED_EDGE ( 'NONE', *, *, #6107, .F. ) ;
#15597 = CARTESIAN_POINT ( 'NONE',  ( -3.500000000000000444, 17.00319992234354416, -0.05647727720529563400 ) ) ;
#15598 = CARTESIAN_POINT ( 'NONE',  ( 2.121784821874994176, -26.01805392422797070, -6.468916616312057499 ) ) ;
#15599 = CARTESIAN_POINT ( 'NONE',  ( 3.481649420246369697, 39.12180007765646650, -1.193696214020541824 ) ) ;
#15600 =( BOUNDED_CURVE ( )  B_SPLINE_CURVE ( 2, ( #8916, #3281, #1899, #16080, #7806, #17670, #13463, #9105, #10679 ),
 .UNSPECIFIED., .F., .T. ) 
 B_SPLINE_CURVE_WITH_KNOTS ( ( 3, 2, 2, 2, 3 ),
 ( 0.9224137931034482873, 0.9252873563218391162, 0.9310344827586206629, 0.9367816091954023205, 0.9396551724137931494 ),
 .UNSPECIFIED. ) 
 CURVE ( )  GEOMETRIC_REPRESENTATION_ITEM ( )  RATIONAL_B_SPLINE_CURVE ( ( 0.9330127018922194093, 0.9330127018922194093, 1.000000000000000000, 0.8660254037844387076, 1.000000000000000000, 0.8660254037844387076, 1.000000000000000000, 0.9330127018922180770, 0.9330127018922194093 ) ) 
 REPRESENTATION_ITEM ( '' )  );
#15601 = CARTESIAN_POINT ( 'NONE',  ( -2.864755990943222308, 34.25319992234354771, 2.011557305968548093 ) ) ;
#15602 = CIRCLE ( 'NONE', #4048, 10.00000000000000000 ) ;
#15603 = DIRECTION ( 'NONE',  ( -1.000000000000000000, 0.000000000000000000, 4.336808689942021680E-16 ) ) ;
#15604 = CARTESIAN_POINT ( 'NONE',  ( 4.730628863548789710E-15, -18.40224968331953548, -10.54263636066531085 ) ) ;
#15605 = DIRECTION ( 'NONE',  ( 1.000000000000000000, 0.000000000000000000, 0.000000000000000000 ) ) ;
#15606 = ADVANCED_FACE ( 'NONE', ( #11650 ), #14352, .F. ) ;
#15607 = CYLINDRICAL_SURFACE ( 'NONE', #16612, 3.799999999999999378 ) ;
#15608 = FACE_OUTER_BOUND ( 'NONE', #17041, .T. ) ;
#15609 = CARTESIAN_POINT ( 'NONE',  ( 4.243569643750000786, -20.12541652831194838, -4.460593432342547793 ) ) ;
#15610 = EDGE_CURVE ( 'NONE', #10059, #3027, #3322, .T. ) ;
#15611 = CARTESIAN_POINT ( 'NONE',  ( -1.661723472263481630E-14, -21.34959095050052014, -13.18268287578030318 ) ) ;
#15612 = CARTESIAN_POINT ( 'NONE',  ( -1.734723475976807094E-15, 16.59999999999999787, -2.500000000000000000 ) ) ;
#15613 = EDGE_LOOP ( 'NONE', ( #8308, #13603, #10081 ) ) ;
#15614 = CARTESIAN_POINT ( 'NONE',  ( -1.593127413382952939, 24.12819992234354771, 2.091722143975172532 ) ) ;
#15615 = EDGE_CURVE ( 'NONE', #6288, #12929, #4701, .T. ) ;
#15616 = CARTESIAN_POINT ( 'NONE',  ( -2.121784821875005722, -29.93271310232382021, -12.05962931858445231 ) ) ;
#15617 = CARTESIAN_POINT ( 'NONE',  ( -2.211161402132902243, 18.37180007765647005, -2.942372952327172886 ) ) ;
#15618 = EDGE_CURVE ( 'NONE', #2949, #4710, #4520, .T. ) ;
#15619 = FACE_OUTER_BOUND ( 'NONE', #12436, .T. ) ;
#15620 = CARTESIAN_POINT ( 'NONE',  ( 9.000000000000005329, -10.00000000000000000, -30.00000000000000000 ) ) ;
#15621 = ORIENTED_EDGE ( 'NONE', *, *, #337, .T. ) ;
#15622 = CARTESIAN_POINT ( 'NONE',  ( -2.121784821875005722, -23.25413247156138397, -2.521627702894468470 ) ) ;
#15623 = CARTESIAN_POINT ( 'NONE',  ( 2.115076519116362963, 28.87180007765647716, -3.012182706137107147 ) ) ;
#15624 = AXIS2_PLACEMENT_3D ( 'NONE', #8680, #17350, #8499 ) ;
#15625 = CIRCLE ( 'NONE', #7618, 2.000000000000001776 ) ;
#15626 =( BOUNDED_CURVE ( )  B_SPLINE_CURVE ( 2, ( #3846, #6711, #12363, #5330, #13002, #2827, #1708, #123, #15611 ),
 .UNSPECIFIED., .F., .F. ) 
 B_SPLINE_CURVE_WITH_KNOTS ( ( 3, 2, 2, 2, 3 ),
 ( 0.3017241379310345306, 0.3045977011494253039, 0.3103448275862069061, 0.3160919540229885083, 0.3189655172413793371 ),
 .UNSPECIFIED. ) 
 CURVE ( )  GEOMETRIC_REPRESENTATION_ITEM ( )  RATIONAL_B_SPLINE_CURVE ( ( 0.9330127018922194093, 0.9330127018922200755, 1.000000000000000000, 0.8660254037844387076, 1.000000000000000000, 0.8660254037844387076, 1.000000000000000000, 0.9330127018922187432, 0.9330127018922194093 ) ) 
 REPRESENTATION_ITEM ( '' )  );
#15627 = CARTESIAN_POINT ( 'NONE',  ( 9.000000000000001776, 43.00000000000000000, -2.500000000000002665 ) ) ;
#15628 = CARTESIAN_POINT ( 'NONE',  ( 4.730628863548789710E-15, -21.72540816142837983, -15.28859851726467589 ) ) ;
#15629 = CARTESIAN_POINT ( 'NONE',  ( 8.499999999999994671, 15.00000000000000178, 20.49999999999999645 ) ) ;
#15630 = CARTESIAN_POINT ( 'NONE',  ( -1.734723475976807094E-15, 27.59999999999999432, -2.500000000000000000 ) ) ;
#15631 = LINE ( 'NONE', #5524, #17424 ) ;
#15632 = CLOSED_SHELL ( 'NONE', ( #9657, #14182, #1113, #9988, #12605, #9146, #789, #15098, #11990, #9769, #5240, #14967, #8565, #15721, #13970, #11703, #2312, #2150, #6589, #4801, #15348, #13278, #16994, #1252, #11750, #8233, #12943, #5902, #14500, #1608, #11464 ) ) ;
#15633 = CARTESIAN_POINT ( 'NONE',  ( 4.243569643750000786, -24.25516687003944938, -10.35848815122331068 ) ) ;
#15634 = DIRECTION ( 'NONE',  ( 0.000000000000000000, 0.000000000000000000, 1.000000000000000000 ) ) ;
#15635 = CARTESIAN_POINT ( 'NONE',  ( 3.999999999999996447, -21.69990767541768761, -2.682881918636178753 ) ) ;
#15636 = AXIS2_PLACEMENT_3D ( 'NONE', #9570, #10595, #17855 ) ;
#15637 = CARTESIAN_POINT ( 'NONE',  ( 1.989345975306426206, 18.99680007765647716, -1.515154207786343799 ) ) ;
#15638 = AXIS2_PLACEMENT_3D ( 'NONE', #9290, #17937, #4848 ) ;
#15639 = ORIENTED_EDGE ( 'NONE', *, *, #3400, .F. ) ;
#15640 = DIRECTION ( 'NONE',  ( 0.000000000000000000, 0.8191520442889952403, -0.5735764363510413855 ) ) ;
#15641 = SURFACE_STYLE_FILL_AREA ( #4046 ) ;
#15642 = CARTESIAN_POINT ( 'NONE',  ( 10.00000000000000355, 16.59999999999999787, 2.499999999999996891 ) ) ;
#15643 = CARTESIAN_POINT ( 'NONE',  ( 0.05938372350921204690, 37.62819992234354771, -2.628655560595669183 ) ) ;
#15644 = ORIENTED_EDGE ( 'NONE', *, *, #11809, .F. ) ;
#15645 = CARTESIAN_POINT ( 'NONE',  ( 4.730628863548789710E-15, -20.46712485418328242, -13.49158372010569096 ) ) ;
#15646 = CARTESIAN_POINT ( 'NONE',  ( 0.05938372350929014415, 32.37180007765647360, 4.731580009072201776 ) ) ;
#15647 = VERTEX_POINT ( 'NONE', #14546 ) ;
#15648 =( LENGTH_UNIT ( ) NAMED_UNIT ( * ) SI_UNIT ( .MILLI., .METRE. ) );
#15649 = CIRCLE ( 'NONE', #12976, 0.9999999999999991118 ) ;
#15650 = CARTESIAN_POINT ( 'NONE',  ( -9.000000000000001776, 23.19999999999999574, 2.499999999999998224 ) ) ;
#15651 = EDGE_CURVE ( 'NONE', #2970, #3053, #15934, .T. ) ;
#15652 = FACE_OUTER_BOUND ( 'NONE', #17621, .T. ) ;
#15653 = CARTESIAN_POINT ( 'NONE',  ( 0.000000000000000000, 5.977523610840987267, 32.81826849749789687 ) ) ;
#15654 = LINE ( 'NONE', #2954, #14744 ) ;
#15655 = CARTESIAN_POINT ( 'NONE',  ( -5.330712181944245322E-15, -25.01042347868947857, -2.894126148162874834 ) ) ;
#15656 = VERTEX_POINT ( 'NONE', #15839 ) ;
#15657 = CARTESIAN_POINT ( 'NONE',  ( -1.734723475976807094E-15, 25.39999999999999503, -2.500000000000000000 ) ) ;
#15658 = EDGE_LOOP ( 'NONE', ( #16819, #10070, #12342, #16131 ) ) ;
#15659 = ORIENTED_EDGE ( 'NONE', *, *, #14847, .F. ) ;
#15660 = CARTESIAN_POINT ( 'NONE',  ( -1.999999999999996225, -17.63731374990092959, -6.946691269403138413 ) ) ;
#15661 = SURFACE_SIDE_STYLE ('',( #1308 ) ) ;
#15662 = FILL_AREA_STYLE ('',( #2461 ) ) ;
#15663 = TOROIDAL_SURFACE ( 'NONE', #7069, 9.000000000000003553, 0.9999999999999991118 ) ;
#15664 = CARTESIAN_POINT ( 'NONE',  ( 1.444289557195957086, 20.25319992234354416, -4.262301884875733471 ) ) ;
#15665 = CARTESIAN_POINT ( 'NONE',  ( -2.211161402132838738, 31.62819992234354416, 2.942372952327218183 ) ) ;
#15666 = CARTESIAN_POINT ( 'NONE',  ( -0.8262555684461330152, 38.49680007765647360, -2.360188852285403982 ) ) ;
#15667 = ORIENTED_EDGE ( 'NONE', *, *, #3201, .T. ) ;
#15668 = B_SPLINE_CURVE_WITH_KNOTS ( 'NONE', 3,
 ( #1463, #12759, #14247, #12931 ),
 .UNSPECIFIED., .F., .F.,
 ( 4, 4 ),
 ( 0.002451451260336424184, 0.003462474391252139301 ),
 .UNSPECIFIED. ) ;
#15669 = CARTESIAN_POINT ( 'NONE',  ( -4.499999999999999112, 32.00319992234354061, -0.05647727720528529505 ) ) ;
#15670 = CARTESIAN_POINT ( 'NONE',  ( 4.000000000000003553, -21.16428301933063949, -9.970566447840647939 ) ) ;
#15671 = ORIENTED_EDGE ( 'NONE', *, *, #10214, .T. ) ;
#15672 = EDGE_CURVE ( 'NONE', #10774, #8639, #10499, .T. ) ;
#15673 = AXIS2_PLACEMENT_3D ( 'NONE', #18340, #4133, #48 ) ;
#15674 = CARTESIAN_POINT ( 'NONE',  ( 4.000000000000000888, -20.81908553137646578, -5.451255436407934418 ) ) ;
#15675 = CIRCLE ( 'NONE', #7666, 3.047499999999999876 ) ;
#15676 = EDGE_CURVE ( 'NONE', #18119, #12399, #12988, .T. ) ;
#15677 = CARTESIAN_POINT ( 'NONE',  ( 2.798362969681366330, 28.99680007765647716, -2.102939460078824929 ) ) ;
#15678 = CYLINDRICAL_SURFACE ( 'NONE', #2222, 0.9999999999999991118 ) ;
#15679 = ADVANCED_FACE ( 'NONE', ( #17149 ), #16809, .F. ) ;
#15680 = CIRCLE ( 'NONE', #12121, 0.9999999999999991118 ) ;
#15681 = CARTESIAN_POINT ( 'NONE',  ( -2.121784821875005722, -26.31918155331226217, -6.898971439563784003 ) ) ;
#15682 = CARTESIAN_POINT ( 'NONE',  ( 4.518350579753633411, 31.87180007765647716, 1.405661355842698468 ) ) ;
#15683 = CARTESIAN_POINT ( 'NONE',  ( -5.577813053751546416E-15, -23.32136551875358776, -2.051094430206859887 ) ) ;
#15684 = EDGE_LOOP ( 'NONE', ( #10146, #8134, #1757, #11488 ) ) ;
#15685 = ORIENTED_EDGE ( 'NONE', *, *, #3781, .T. ) ;
#15686 = CARTESIAN_POINT ( 'NONE',  ( 3.518350579753631191, 26.87180007765647360, 1.080741659609802285 ) ) ;
#15687 = DIRECTION ( 'NONE',  ( -0.000000000000000000, -1.000000000000000000, -0.000000000000000000 ) ) ;
#15688 = DIRECTION ( 'NONE',  ( 0.000000000000000000, 0.000000000000000000, -1.000000000000000000 ) ) ;
#15689 = VERTEX_POINT ( 'NONE', #3505 ) ;
#15690 = CARTESIAN_POINT ( 'NONE',  ( 3.481649420246394122, 18.37819992234354771, 1.193696214020467439 ) ) ;
#15691 = CARTESIAN_POINT ( 'NONE',  ( -4.243569643750005227, -25.07910933890011407, -7.263709834155468670 ) ) ;
#15692 = CARTESIAN_POINT ( 'NONE',  ( -2.864755990943265829, 35.74680007765648071, -2.011557305968488141 ) ) ;
#15693 = AXIS2_PLACEMENT_3D ( 'NONE', #8007, #16840, #15349 ) ;
#15694 = CARTESIAN_POINT ( 'NONE',  ( 0.05938372350920109732, 37.62819992234352640, -3.680117784833935701 ) ) ;
#15695 = DIRECTION ( 'NONE',  ( 1.000000000000000000, 0.000000000000000000, -0.000000000000000000 ) ) ;
#15696 = AXIS2_PLACEMENT_3D ( 'NONE', #2857, #4514, #12583 ) ;
#15697 = CARTESIAN_POINT ( 'NONE',  ( 4.243569643750003451, -21.22653997395446623, -10.30465079805533435 ) ) ;
#15698 = CARTESIAN_POINT ( 'NONE',  ( -6.079313232897520791, -14.44302855110153594, -4.023496914806315772 ) ) ;
#15699 = AXIS2_PLACEMENT_3D ( 'NONE', #10454, #10356, #7484 ) ;
#15700 = CARTESIAN_POINT ( 'NONE',  ( 0.000000000000000000, 5.977523610840987267, 32.81826849749789687 ) ) ;
#15701 = DIRECTION ( 'NONE',  ( -1.000000000000000000, -0.000000000000000000, -0.000000000000000000 ) ) ;
#15702 =( BOUNDED_CURVE ( )  B_SPLINE_CURVE ( 2, ( #6018, #14474, #2799, #8429, #15674, #12697, #14093, #5655, #9999 ),
 .UNSPECIFIED., .F., .T. ) 
 B_SPLINE_CURVE_WITH_KNOTS ( ( 3, 2, 2, 2, 3 ),
 ( 0.8189655172413793371, 0.8218390804597701660, 0.8275862068965517127, 0.8333333333333333703, 0.8362068965517241992 ),
 .UNSPECIFIED. ) 
 CURVE ( )  GEOMETRIC_REPRESENTATION_ITEM ( )  RATIONAL_B_SPLINE_CURVE ( ( 0.9330127018922194093, 0.9330127018922194093, 1.000000000000000000, 0.8660254037844387076, 1.000000000000000000, 0.8660254037844387076, 1.000000000000000000, 0.9330127018922180770, 0.9330127018922194093 ) ) 
 REPRESENTATION_ITEM ( '' )  );
#15703 = CARTESIAN_POINT ( 'NONE',  ( -2.121784821874996396, -17.28707365596521939, -6.814254884211938368 ) ) ;
#15704 = CARTESIAN_POINT ( 'NONE',  ( 8.500000000000019540, 0.000000000000000000, -18.49999999999998934 ) ) ;
#15705 = SURFACE_STYLE_FILL_AREA ( #12906 ) ;
#15706 = ORIENTED_EDGE ( 'NONE', *, *, #7265, .T. ) ;
#15707 = CARTESIAN_POINT ( 'NONE',  ( 2.500000000000001332, 18.25319992234354771, 0.05647727720530566764 ) ) ;
#15708 = CARTESIAN_POINT ( 'NONE',  ( -4.000000000000004441, -24.04440135829761616, -6.031165898660685976 ) ) ;
#15709 = DIRECTION ( 'NONE',  ( 1.000000000000000000, 0.000000000000000000, 0.000000000000000000 ) ) ;
#15710 = CARTESIAN_POINT ( 'NONE',  ( 8.000000000000000000, 27.59999999999999432, -2.500000000000000888 ) ) ;
#15711 = DIRECTION ( 'NONE',  ( -0.000000000000000000, -0.5735764363510414965, -0.8191520442889950182 ) ) ;
#15712 = ORIENTED_EDGE ( 'NONE', *, *, #2383, .T. ) ;
#15713 = CARTESIAN_POINT ( 'NONE',  ( -4.243569643750004339, -22.01406025714923587, -2.886366097486154469 ) ) ;
#15714 = AXIS2_PLACEMENT_3D ( 'NONE', #1365, #56, #2845 ) ;
#15715 = CARTESIAN_POINT ( 'NONE',  ( -2.864755990943265829, 33.24680007765648071, -2.011557305968488141 ) ) ;
#15716 = CARTESIAN_POINT ( 'NONE',  ( 4.243569643750000786, -26.61041511180591357, -13.72213123308499760 ) ) ;
#15717 = EDGE_CURVE ( 'NONE', #9679, #7045, #10449, .T. ) ;
#15718 = CYLINDRICAL_SURFACE ( 'NONE', #16348, 0.9999999999999991118 ) ;
#15719 = CARTESIAN_POINT ( 'NONE',  ( 4.243569643750000786, -25.02949505911335137, -11.46434341101345389 ) ) ;
#15720 = CARTESIAN_POINT ( 'NONE',  ( 8.500000000000019540, 0.000000000000000000, 22.49999999999999289 ) ) ;
#15721 = ADVANCED_FACE ( 'NONE', ( #13327 ), #16398, .F. ) ;
#15722 = CARTESIAN_POINT ( 'NONE',  ( 1.533898589781675205E-14, -27.77375260663349366, -8.409762175006950002 ) ) ;
#15723 = DIRECTION ( 'NONE',  ( 0.000000000000000000, 0.000000000000000000, -1.000000000000000000 ) ) ;
#15724 = CARTESIAN_POINT ( 'NONE',  ( 4.243569643750003451, -23.00104207391549593, -12.83890243507441120 ) ) ;
#15725 = CARTESIAN_POINT ( 'NONE',  ( -9.000000000000003553, 29.79999999999999716, -2.500000000000001776 ) ) ;
#15726 = CARTESIAN_POINT ( 'NONE',  ( 4.000000000000003553, -18.64771640554539545, -6.376536854529448739 ) ) ;
#15727 = VECTOR ( 'NONE', #3749, 1000.000000000000000 ) ;
#15728 = CARTESIAN_POINT ( 'NONE',  ( -2.481649420246374138, 22.87180007765648071, 0.8687765177876256573 ) ) ;
#15729 = ORIENTED_EDGE ( 'NONE', *, *, #2770, .T. ) ;
#15730 = CARTESIAN_POINT ( 'NONE',  ( -2.864755990943265829, 18.24680007765648071, -2.011557305968488141 ) ) ;
#15731 = DIRECTION ( 'NONE',  ( -0.000000000000000000, -1.000000000000000000, -0.000000000000000000 ) ) ;
#15732 = DIRECTION ( 'NONE',  ( 0.000000000000000000, 0.000000000000000000, 1.000000000000000000 ) ) ;
#15733 = CARTESIAN_POINT ( 'NONE',  ( 0.000000000000000000, 9.254131787996968228, 30.52396275209373044 ) ) ;
#15734 = CARTESIAN_POINT ( 'NONE',  ( 2.518350579753611207, 33.12819992234354771, -0.7558219633769606149 ) ) ;
#15735 =( BOUNDED_CURVE ( )  B_SPLINE_CURVE ( 2, ( #869, #18222, #17941, #11052, #9294, #6691, #6516, #3917, #10777 ),
 .UNSPECIFIED., .F., .F. ) 
 B_SPLINE_CURVE_WITH_KNOTS ( ( 3, 2, 2, 2, 3 ),
 ( 0.7155172413793103869, 0.7183908045977011048, 0.7241379310344827624, 0.7298850574712644201, 0.7327586206896552490 ),
 .UNSPECIFIED. ) 
 CURVE ( )  GEOMETRIC_REPRESENTATION_ITEM ( )  RATIONAL_B_SPLINE_CURVE ( ( 0.9330127018922194093, 0.9330127018922206306, 1.000000000000000000, 0.8660254037844387076, 1.000000000000000000, 0.8660254037844387076, 1.000000000000000000, 0.9330127018922180770, 0.9330127018922194093 ) ) 
 REPRESENTATION_ITEM ( '' )  );
#15736 = ORIENTED_EDGE ( 'NONE', *, *, #18236, .F. ) ;
#15737 = CARTESIAN_POINT ( 'NONE',  ( 2.121784821875004390, -21.49210590496380036, -12.81966330890563022 ) ) ;
#15738 = CARTESIAN_POINT ( 'NONE',  ( 4.499999999999999112, 31.74680007765647716, -0.05647727720537982360 ) ) ;
#15739 = ORIENTED_EDGE ( 'NONE', *, *, #9598, .F. ) ;
#15740 = MECHANICAL_DESIGN_GEOMETRIC_PRESENTATION_REPRESENTATION (  '', ( #12185 ), #1541 ) ;
#15741 = FILL_AREA_STYLE_COLOUR ( '', #903 ) ;
#15742 = EDGE_CURVE ( 'NONE', #17338, #4165, #1470, .T. ) ;
#15743 = CARTESIAN_POINT ( 'NONE',  ( 4.299564228933482956E-15, -19.47829782620029704, -10.51019933028069708 ) ) ;
#15744 = DIRECTION ( 'NONE',  ( 0.000000000000000000, 0.000000000000000000, 1.000000000000000000 ) ) ;
#15745 = CARTESIAN_POINT ( 'NONE',  ( 4.898587196589415787E-16, 3.000000000000000000, -4.000000000000001776 ) ) ;
#15746 = DIRECTION ( 'NONE',  ( 3.469446951953612217E-16, -0.000000000000000000, 1.000000000000000000 ) ) ;
#15747 = CARTESIAN_POINT ( 'NONE',  ( -2.121784821875005722, -24.28657005699325921, -3.996101382614658970 ) ) ;
#15748 = ORIENTED_EDGE ( 'NONE', *, *, #3864, .T. ) ;
#15749 = VECTOR ( 'NONE', #15898, 1000.000000000000000 ) ;
#15750 = CARTESIAN_POINT ( 'NONE',  ( 3.999999999999996447, -24.99080247827684431, -7.382766771737522049 ) ) ;
#15751 = ORIENTED_EDGE ( 'NONE', *, *, #9883, .F. ) ;
#15752 = ORIENTED_EDGE ( 'NONE', *, *, #3565, .T. ) ;
#15753 = LINE ( 'NONE', #14174, #10758 ) ;
#15754 = CARTESIAN_POINT ( 'NONE',  ( -3.706921591972381904E-14, -17.67153205169451624, -7.929870390770359379 ) ) ;
#15755 = FILL_AREA_STYLE_COLOUR ( '', #6274 ) ;
#15756 = CARTESIAN_POINT ( 'NONE',  ( 1.336863392178569754, 18.75319992234354416, 4.297206761780648421 ) ) ;
#15757 = CARTESIAN_POINT ( 'NONE',  ( -2.211161402132838738, 29.12819992234354416, 2.942372952327218183 ) ) ;
#15758 = CARTESIAN_POINT ( 'NONE',  ( -1.497042530366522461, 14.87819992234354594, -2.161531897785030409 ) ) ;
#15759 = VERTEX_POINT ( 'NONE', #9330 ) ;
#15760 = CARTESIAN_POINT ( 'NONE',  ( -4.481649420246396787, 34.62819992234354771, -1.518615910253363399 ) ) ;
#15761 = CARTESIAN_POINT ( 'NONE',  ( 4.000000000000000888, -23.07754274880374368, -8.676666609789087659 ) ) ;
#15762 = ORIENTED_EDGE ( 'NONE', *, *, #10207, .F. ) ;
#15763 = VECTOR ( 'NONE', #4987, 1000.000000000000000 ) ;
#15764 = CYLINDRICAL_SURFACE ( 'NONE', #11475, 4.000000000000000000 ) ;
#15765 = AXIS2_PLACEMENT_3D ( 'NONE', #6315, #7696, #13260 ) ;
#15766 = CARTESIAN_POINT ( 'NONE',  ( 3.481649420246369697, 31.62180007765647360, -1.193696214020541824 ) ) ;
#15767 = CARTESIAN_POINT ( 'NONE',  ( -6.616789018075169615, -14.16315581186571571, -2.134625489590734837 ) ) ;
#15768 = CARTESIAN_POINT ( 'NONE',  ( -2.121784821874996396, -18.57762063775506078, -8.657346983862177936 ) ) ;
#15769 = CARTESIAN_POINT ( 'NONE',  ( -2.733110507866247652, 30.12180007765647716, 3.862833514489154574 ) ) ;
#15770 = CARTESIAN_POINT ( 'NONE',  ( 0.000000000000000000, 15.00000000000000355, 0.000000000000000000 ) ) ;
#15771 = VERTEX_POINT ( 'NONE', #15007 ) ;
#15772 = ORIENTED_EDGE ( 'NONE', *, *, #14377, .T. ) ;
#15773 = CARTESIAN_POINT ( 'NONE',  ( 1.135272562821090458, 19.74680007765648071, 3.311245368580554072 ) ) ;
#15774 = CARTESIAN_POINT ( 'NONE',  ( -4.000000000000004441, -25.07683894372948785, -7.505639578380876031 ) ) ;
#15775 = EDGE_CURVE ( 'NONE', #10347, #12347, #7080, .T. ) ;
#15776 = DIRECTION ( 'NONE',  ( -0.000000000000000000, -1.000000000000000000, -0.000000000000000000 ) ) ;
#15777 = VECTOR ( 'NONE', #4741, 1000.000000000000000 ) ;
#15778 = CARTESIAN_POINT ( 'NONE',  ( 1.999999999999994449, -23.95783908012565888, -3.894383200091054320 ) ) ;
#15779 = ORIENTED_EDGE ( 'NONE', *, *, #16928, .F. ) ;
#15780 = VECTOR ( 'NONE', #14382, 1000.000000000000114 ) ;
#15781 = CARTESIAN_POINT ( 'NONE',  ( -0.05938372350920063936, 21.37819992234353705, 3.680117784833935701 ) ) ;
#15782 = EDGE_CURVE ( 'NONE', #94, #5846, #13096, .T. ) ;
#15783 = CARTESIAN_POINT ( 'NONE',  ( -1.734723475976807094E-15, 20.99999999999999289, -11.50000000000000178 ) ) ;
#15784 = CARTESIAN_POINT ( 'NONE',  ( 4.243569643749996345, -25.25118226980542602, -7.509455447442161535 ) ) ;
#15785 = CARTESIAN_POINT ( 'NONE',  ( -0.8262555684461330152, 15.99680007765648249, -2.360188852285403982 ) ) ;
#15786 = APPLICATION_CONTEXT ( 'automotive_design' ) ;
#15787 = EDGE_CURVE ( 'NONE', #8354, #8879, #18252, .T. ) ;
#15788 = CARTESIAN_POINT ( 'NONE',  ( 0.05938372350920109732, 32.62819992234354771, -3.680117784833935701 ) ) ;
#15789 = LINE ( 'NONE', #8717, #8148 ) ;
#15790 = DIRECTION ( 'NONE',  ( 0.000000000000000000, 0.000000000000000000, -1.000000000000000000 ) ) ;
#15791 = ADVANCED_FACE ( 'NONE', ( #18344 ), #4037, .T. ) ;
#15792 = CARTESIAN_POINT ( 'NONE',  ( 4.243569643749996345, -24.50911775527627157, -6.449677490143276515 ) ) ;
#15793 = DIRECTION ( 'NONE',  ( -0.000000000000000000, -0.000000000000000000, -1.000000000000000000 ) ) ;
#15794 = CIRCLE ( 'NONE', #4534, 0.9999999999999991118 ) ;
#15795 = UNCERTAINTY_MEASURE_WITH_UNIT (LENGTH_MEASURE( 1.000000000000000082E-05 ), #11823, 'distance_accuracy_value', 'NONE');
#15796 = EDGE_CURVE ( 'NONE', #6366, #9679, #16885, .T. ) ;
#15797 = DIRECTION ( 'NONE',  ( 0.000000000000000000, 0.000000000000000000, -1.000000000000000000 ) ) ;
#15798 = CARTESIAN_POINT ( 'NONE',  ( 8.500000000000001776, 13.00000000000000178, -18.35000000000000142 ) ) ;
#15799 = DIRECTION ( 'NONE',  ( 3.469446951953612217E-16, -0.000000000000000000, 1.000000000000000000 ) ) ;
#15800 = CARTESIAN_POINT ( 'NONE',  ( 4.243569643750003451, -18.87129173218799849, -6.941007716193646537 ) ) ;
#15801 = CARTESIAN_POINT ( 'NONE',  ( -2.238531268403934682, 15.00000000000000355, -2.169313016320178367 ) ) ;
#15802 = ORIENTED_EDGE ( 'NONE', *, *, #11179, .F. ) ;
#15803 = CARTESIAN_POINT ( 'NONE',  ( -1.593127413382952939, 21.62819992234354416, 2.091722143975172532 ) ) ;
#15804 = CARTESIAN_POINT ( 'NONE',  ( 4.730628863548789710E-15, -23.01595514321822122, -17.13169061691491279 ) ) ;
#15805 = DIRECTION ( 'NONE',  ( 3.469446951953612217E-16, -0.000000000000000000, 1.000000000000000000 ) ) ;
#15806 = AXIS2_PLACEMENT_3D ( 'NONE', #11252, #4126, #1352 ) ;
#15807 = CARTESIAN_POINT ( 'NONE',  ( -4.518350579753602325, 39.37819992234354771, 1.405661355842794391 ) ) ;
#15808 = CARTESIAN_POINT ( 'NONE',  ( -9.974462289245280999, -9.920488278021490913, 4.137459934542836670 ) ) ;
#15809 = CARTESIAN_POINT ( 'NONE',  ( -15.00000000000000178, 13.00000000000000178, -25.00000000000000355 ) ) ;
#15810 = EDGE_LOOP ( 'NONE', ( #11523, #1570, #17819, #83 ) ) ;
#15811 = CARTESIAN_POINT ( 'NONE',  ( 2.121784821874994176, -22.69489544611912279, -1.722954459712693787 ) ) ;
#15812 = CARTESIAN_POINT ( 'NONE',  ( 2.115076519116362963, 33.87180007765648071, -3.012182706137107147 ) ) ;
#15813 = CARTESIAN_POINT ( 'NONE',  ( 4.713407268011036227E-15, -16.13220141719875400, -6.810327045070806662 ) ) ;
#15814 = DIRECTION ( 'NONE',  ( -0.000000000000000000, -0.5735764363510414965, -0.8191520442889950182 ) ) ;
#15815 = CARTESIAN_POINT ( 'NONE',  ( 4.243569643750003451, -23.00104207391549593, -12.83890243507440942 ) ) ;
#15816 =( BOUNDED_CURVE ( )  B_SPLINE_CURVE ( 2, ( #8815, #5769, #17016, #1515, #14212, #4468, #7148, #7331, #2995 ),
 .UNSPECIFIED., .F., .F. ) 
 B_SPLINE_CURVE_WITH_KNOTS ( ( 3, 2, 2, 2, 3 ),
 ( 0.2672413793103448620, 0.2701149425287356354, 0.2758620689655172376, 0.2816091954022988397, 0.2844827586206896686 ),
 .UNSPECIFIED. ) 
 CURVE ( )  GEOMETRIC_REPRESENTATION_ITEM ( )  RATIONAL_B_SPLINE_CURVE ( ( 0.9330127018922194093, 0.9330127018922200755, 1.000000000000000000, 0.8660254037844387076, 1.000000000000000000, 0.8660254037844387076, 1.000000000000000000, 0.9330127018922187432, 0.9330127018922194093 ) ) 
 REPRESENTATION_ITEM ( '' )  );
#15817 = CYLINDRICAL_SURFACE ( 'NONE', #11733, 4.000000000000000000 ) ;
#15818 = DIRECTION ( 'NONE',  ( 0.000000000000000000, -1.000000000000000000, 0.000000000000000000 ) ) ;
#15819 = EDGE_CURVE ( 'NONE', #5664, #5122, #11812, .T. ) ;
#15820 = DIRECTION ( 'NONE',  ( -3.469446951953613696E-16, -0.000000000000000000, -1.000000000000000000 ) ) ;
#15821 = CARTESIAN_POINT ( 'NONE',  ( -4.243569643750000786, -24.38422156821842535, -10.54279736118833988 ) ) ;
#15822 = CARTESIAN_POINT ( 'NONE',  ( 0.000000000000000000, 9.254131787996968228, 30.52396275209373044 ) ) ;
#15823 = CARTESIAN_POINT ( 'NONE',  ( 3.999999999999996447, -22.47423586449159671, -3.788737178426322849 ) ) ;
#15824 = CARTESIAN_POINT ( 'NONE',  ( 1.497042530366477164, 23.87180007765647716, -2.161531897785062384 ) ) ;
#15825 = ORIENTED_EDGE ( 'NONE', *, *, #10792, .F. ) ;
#15826 = CARTESIAN_POINT ( 'NONE',  ( 2.115076519116362963, 18.87180007765648071, -3.012182706137107591 ) ) ;
#15827 = CARTESIAN_POINT ( 'NONE',  ( 4.000000000000000000, 1.759474945355381514, -3.047500000000001652 ) ) ;
#15828 = DIRECTION ( 'NONE',  ( 1.000000000000000000, 0.000000000000000000, 0.000000000000000000 ) ) ;
#15829 = CARTESIAN_POINT ( 'NONE',  ( 3.375445829055900404, -25.20600189401019264, -15.83707978931157534 ) ) ;
#15830 = CARTESIAN_POINT ( 'NONE',  ( -2.864755990943222308, 21.75319992234354771, 2.011557305968548093 ) ) ;
#15831 = VERTEX_POINT ( 'NONE', #14141 ) ;
#15832 = CARTESIAN_POINT ( 'NONE',  ( -4.243569643750004339, -25.62759180616079746, -8.047023976506819665 ) ) ;
#15833 = CARTESIAN_POINT ( 'NONE',  ( -0.05938372350928957516, 36.12180007765646650, -4.731580009072201776 ) ) ;
#15834 = ORIENTED_EDGE ( 'NONE', *, *, #12879, .T. ) ;
#15835 =( LENGTH_UNIT ( ) NAMED_UNIT ( * ) SI_UNIT ( .MILLI., .METRE. ) );
#15836 = LINE ( 'NONE', #17243, #1765 ) ;
#15837 = CARTESIAN_POINT ( 'NONE',  ( 2.121784821875004390, -22.00832469767973620, -13.55690014876572569 ) ) ;
#15838 = CARTESIAN_POINT ( 'NONE',  ( 10.00000000000000355, 36.39999999999999147, 2.499999999999996891 ) ) ;
#15839 = CARTESIAN_POINT ( 'NONE',  ( 13.00000000000000178, 49.00000000000000000, 16.00000000000000000 ) ) ;
#15840 = CARTESIAN_POINT ( 'NONE',  ( 4.000000000000003553, -20.64806422661470720, -9.233329607980554243 ) ) ;
#15841 = CARTESIAN_POINT ( 'NONE',  ( 4.243569643749996345, -23.99289896256033572, -5.712440650283179266 ) ) ;
#15842 = ORIENTED_EDGE ( 'NONE', *, *, #6941, .F. ) ;
#15843 = EDGE_CURVE ( 'NONE', #13521, #14942, #1455, .T. ) ;
#15844 = FACE_OUTER_BOUND ( 'NONE', #2184, .T. ) ;
#15845 = DIRECTION ( 'NONE',  ( 0.000000000000000000, 0.000000000000000000, -1.000000000000000000 ) ) ;
#15846 = ORIENTED_EDGE ( 'NONE', *, *, #14416, .T. ) ;
#15847 = ORIENTED_EDGE ( 'NONE', *, *, #13245, .T. ) ;
#15848 = DIRECTION ( 'NONE',  ( -1.000000000000000000, -0.000000000000000000, -0.000000000000000000 ) ) ;
#15849 = CARTESIAN_POINT ( 'NONE',  ( 10.00000000000000000, 18.79999999999999361, -2.500000000000003109 ) ) ;
#15850 = CARTESIAN_POINT ( 'NONE',  ( 2.733110507866328920, 28.62819992234354416, 3.862833514489095510 ) ) ;
#15851 = CARTESIAN_POINT ( 'NONE',  ( -3.518350579753606322, 29.37819992234354771, 1.080741659609877781 ) ) ;
#15852 = EDGE_CURVE ( 'NONE', #12298, #14652, #14191, .T. ) ;
#15853 = CARTESIAN_POINT ( 'NONE',  ( 2.500000000000001332, 39.24680007765647360, -0.05647727720535888202 ) ) ;
#15854 = ORIENTED_EDGE ( 'NONE', *, *, #11573, .T. ) ;
#15855 = CARTESIAN_POINT ( 'NONE',  ( 1.444289557195957086, 30.25319992234354061, -4.262301884875733471 ) ) ;
#15856 = EDGE_CURVE ( 'NONE', #18310, #14557, #16921, .T. ) ;
#15857 = CARTESIAN_POINT ( 'NONE',  ( -4.000000000000000888, -23.98092563605662875, -9.966831079544254735 ) ) ;
#15858 = ORIENTED_EDGE ( 'NONE', *, *, #12314, .T. ) ;
#15859 = DIRECTION ( 'NONE',  ( -0.000000000000000000, 1.000000000000000000, -0.000000000000000000 ) ) ;
#15860 = CARTESIAN_POINT ( 'NONE',  ( 3.481649420246369697, 26.62180007765648071, -1.193696214020541824 ) ) ;
#15861 = CARTESIAN_POINT ( 'NONE',  ( -10.00496734058828174, -9.915240373983317923, 7.344972601042156768 ) ) ;
#15862 = CARTESIAN_POINT ( 'NONE',  ( -5.330712181944246111E-15, -26.01059738957659917, -4.322522525391808479 ) ) ;
#15863 = TOROIDAL_SURFACE ( 'NONE', #7859, 9.000000000000003553, 0.9999999999999991118 ) ;
#15864 = CARTESIAN_POINT ( 'NONE',  ( 1.336863392178479160, 28.74680007765647360, -4.297206761780677731 ) ) ;
#15865 = CARTESIAN_POINT ( 'NONE',  ( -1.734723475976807094E-15, 36.39999999999999147, -2.500000000000000000 ) ) ;
#15866 = ORIENTED_EDGE ( 'NONE', *, *, #13795, .T. ) ;
#15867 = VERTEX_POINT ( 'NONE', #9783 ) ;
#15868 = SHAPE_REPRESENTATION ( 'MAS-178', ( #8940, #5092, #11598, #15182, #8349, #13392, #16075, #16367, #367, #14892, #11020, #4496, #2742, #7160 ), #5407 ) ;
#15869 = CARTESIAN_POINT ( 'NONE',  ( 1.027846397803542144, 28.74680007765647716, -3.346150245485522312 ) ) ;
#15870 = DIRECTION ( 'NONE',  ( -0.000000000000000000, -1.000000000000000000, -0.000000000000000000 ) ) ;
#15871 = CARTESIAN_POINT ( 'NONE',  ( -1.734723475976807094E-15, 23.19999999999999574, -2.500000000000000000 ) ) ;
#15872 = CARTESIAN_POINT ( 'NONE',  ( -3.706921591972381904E-14, -17.47795000513098884, -7.653406576829588026 ) ) ;
#15873 = CARTESIAN_POINT ( 'NONE',  ( 4.000000000000003553, -22.97104879383642384, -12.55089538735098387 ) ) ;
#15874 = ORIENTED_EDGE ( 'NONE', *, *, #11579, .T. ) ;
#15875 = CARTESIAN_POINT ( 'NONE',  ( 2.115076519116426024, 18.62819992234354771, 3.012182706137062294 ) ) ;
#15876 = CARTESIAN_POINT ( 'NONE',  ( -4.243569643750000786, -21.54501820828076930, -6.487994741957813005 ) ) ;
#15877 = CARTESIAN_POINT ( 'NONE',  ( -1.497042530366477164, 17.62180007765648071, 2.161531897785062384 ) ) ;
#15878 = CARTESIAN_POINT ( 'NONE',  ( -3.518350579753605434, 34.37819992234354771, 1.080741659609877781 ) ) ;
#15879 = CARTESIAN_POINT ( 'NONE',  ( -5.330712181944246111E-15, -30.94693959492275681, -11.37234980655397187 ) ) ;
#15880 = CARTESIAN_POINT ( 'NONE',  ( -8.500000000000005329, 10.00000000000000000, -22.64999999999999147 ) ) ;
#15881 = AXIS2_PLACEMENT_3D ( 'NONE', #5320, #13755, #15341 ) ;
#15882 = CARTESIAN_POINT ( 'NONE',  ( 2.121784821875004390, -20.20155892317395541, -10.97657120925539154 ) ) ;
#15883 = CARTESIAN_POINT ( 'NONE',  ( -7.496011132626526852, -13.00850824371983272, 4.993358875981036782 ) ) ;
#15884 = EDGE_CURVE ( 'NONE', #3649, #8594, #12750, .T. ) ;
#15885 = ADVANCED_FACE ( 'NONE', ( #16858 ), #16949, .T. ) ;
#15886 = CARTESIAN_POINT ( 'NONE',  ( -7.951672694476823011, -10.00000000000000178, -6.265341990738099831 ) ) ;
#15887 = DIRECTION ( 'NONE',  ( -3.469446951953613696E-16, -0.000000000000000000, -1.000000000000000000 ) ) ;
#15888 = CARTESIAN_POINT ( 'NONE',  ( 9.000000000000005329, 18.79999999999999361, 2.499999999999997335 ) ) ;
#15889 = VERTEX_POINT ( 'NONE', #5523 ) ;
#15890 = ORIENTED_EDGE ( 'NONE', *, *, #16149, .T. ) ;
#15891 = CARTESIAN_POINT ( 'NONE',  ( -5.330712181944245322E-15, -24.72005040778675777, -2.479430425741570243 ) ) ;
#15892 = FACE_OUTER_BOUND ( 'NONE', #11791, .T. ) ;
#15893 = FACE_BOUND ( 'NONE', #11400, .T. ) ;
#15894 = ORIENTED_EDGE ( 'NONE', *, *, #9101, .T. ) ;
#15895 = CARTESIAN_POINT ( 'NONE',  ( -2.500000000000001332, 19.50319992234354771, -0.05647727720530596601 ) ) ;
#15896 = TOROIDAL_SURFACE ( 'NONE', #2590, 9.000000000000001776, 0.9999999999999991118 ) ;
#15897 = CARTESIAN_POINT ( 'NONE',  ( 4.243569643749996345, -28.86471381881699116, -12.67011332646282895 ) ) ;
#15898 = DIRECTION ( 'NONE',  ( 0.000000000000000000, 0.000000000000000000, 1.000000000000000000 ) ) ;
#15899 = CARTESIAN_POINT ( 'NONE',  ( 0.000000000000000000, 9.254131787996968228, 30.52396275209373044 ) ) ;
#15900 = CARTESIAN_POINT ( 'NONE',  ( -1.734723475976807094E-15, 25.39999999999999503, -11.50000000000000178 ) ) ;
#15901 = ORIENTED_EDGE ( 'NONE', *, *, #9929, .F. ) ;
#15902 = CARTESIAN_POINT ( 'NONE',  ( -2.115076519116362519, 40.12180007765648071, 3.012182706137107147 ) ) ;
#15903 = CARTESIAN_POINT ( 'NONE',  ( -2.121784821875005722, -29.96497677686856775, -12.10570662107570961 ) ) ;
#15904 = EDGE_CURVE ( 'NONE', #10307, #16888, #16579, .T. ) ;
#15905 = EDGE_CURVE ( 'NONE', #13681, #10807, #2925, .T. ) ;
#15906 = CARTESIAN_POINT ( 'NONE',  ( -9.184850993605147944E-16, 13.00000000000000178, -2.500000000000000000 ) ) ;
#15907 = EDGE_CURVE ( 'NONE', #18076, #14905, #15278, .T. ) ;
#15908 = CIRCLE ( 'NONE', #13825, 0.1999999999999987899 ) ;
#15909 = CARTESIAN_POINT ( 'NONE',  ( 4.243569643750000786, -26.32004204090319632, -13.30743551066369257 ) ) ;
#15910 = CARTESIAN_POINT ( 'NONE',  ( -1.999999999999996225, -21.76706409162843059, -12.84458598828390130 ) ) ;
#15911 = FACE_OUTER_BOUND ( 'NONE', #13433, .T. ) ;
#15912 = CARTESIAN_POINT ( 'NONE',  ( -5.330712181944245322E-15, -28.33358195679831937, -7.640088304762238103 ) ) ;
#15913 = CARTESIAN_POINT ( 'NONE',  ( -5.577813053751546416E-15, -25.19265864305380376, -4.723577975706471754 ) ) ;
#15914 = CARTESIAN_POINT ( 'NONE',  ( 4.713407268011036227E-15, -16.19672876699319630, -6.902481651060079493 ) ) ;
#15915 = CARTESIAN_POINT ( 'NONE',  ( 1.497042530366477164, 26.37180007765647716, -2.161531897785062384 ) ) ;
#15916 = ORIENTED_EDGE ( 'NONE', *, *, #1176, .T. ) ;
#15917 = CARTESIAN_POINT ( 'NONE',  ( -3.518350579753630303, 20.62180007765647360, -1.080741659609802952 ) ) ;
#15918 = CARTESIAN_POINT ( 'NONE',  ( 4.000000000000003553, -22.00313855819898379, -11.16857631362007020 ) ) ;
#15919 = DIRECTION ( 'NONE',  ( 0.000000000000000000, 0.000000000000000000, 1.000000000000000000 ) ) ;
#15920 = CIRCLE ( 'NONE', #1156, 8.000000000000001776 ) ;
#15921 = CARTESIAN_POINT ( 'NONE',  ( -5.279047395330986450E-15, -29.82930203384519530, -10.26654236056660352 ) ) ;
#15922 = DIRECTION ( 'NONE',  ( 1.000000000000000000, 0.000000000000000000, 0.000000000000000000 ) ) ;
#15923 = AXIS2_PLACEMENT_3D ( 'NONE', #6993, #9957, #7086 ) ;
#15924 = CARTESIAN_POINT ( 'NONE',  ( -3.481649420246394122, 19.62819992234354416, -1.193696214020467883 ) ) ;
#15925 = ORIENTED_EDGE ( 'NONE', *, *, #10393, .T. ) ;
#15926 = CARTESIAN_POINT ( 'NONE',  ( 4.243569643750003451, -21.48464937031243238, -10.67326921798538031 ) ) ;
#15927 = CARTESIAN_POINT ( 'NONE',  ( -3.481649420246369697, 17.87180007765648071, 1.193696214020542490 ) ) ;
#15928 = ORIENTED_EDGE ( 'NONE', *, *, #9660, .T. ) ;
#15929 = CARTESIAN_POINT ( 'NONE',  ( 4.000000000000003553, -19.61562664118283195, -7.758855928260365076 ) ) ;
#15930 = DIRECTION ( 'NONE',  ( -1.000000000000000000, 0.000000000000000000, 4.336808689942021680E-16 ) ) ;
#15931 = CARTESIAN_POINT ( 'NONE',  ( 2.121784821874994176, -28.37330216599443489, -9.832559698173744422 ) ) ;
#15932 = FACE_OUTER_BOUND ( 'NONE', #1884, .T. ) ;
#15933 = CIRCLE ( 'NONE', #8807, 2.200000000000000622 ) ;
#15934 = LINE ( 'NONE', #3232, #2077 ) ;
#15936 = DIRECTION ( 'NONE',  ( 0.000000000000000000, -1.000000000000000000, 0.000000000000000000 ) ) ;
#15935 = VECTOR ( 'NONE', #11244, 1000.000000000000000 ) ;
#15937 = CARTESIAN_POINT ( 'NONE',  ( -5.330712181944245322E-15, -25.78475166776338412, -3.999981407953017598 ) ) ;
#15938 = ORIENTED_EDGE ( 'NONE', *, *, #16603, .F. ) ;
#15939 = CARTESIAN_POINT ( 'NONE',  ( 1.999999999999994449, -22.40918270197784778, -1.682672680510768792 ) ) ;
#15940 = EDGE_CURVE ( 'NONE', #3198, #1402, #6793, .T. ) ;
#15941 = DIRECTION ( 'NONE',  ( 0.000000000000000000, 0.000000000000000000, -1.000000000000000000 ) ) ;
#15942 = SPHERICAL_SURFACE ( 'NONE', #4077, 4.324969328314201000 ) ;
#15943 = EDGE_LOOP ( 'NONE', ( #16607, #3293, #3259, #15046, #6030, #499, #4936, #11105, #3401, #5075, #7536, #12100, #16447, #1906, #3070, #657, #10702, #4302, #1477, #576, #11870, #4323, #13584, #3680, #10863, #5193, #16565, #11486, #1848, #6407, #7893, #9115, #16774, #13837, #14964, #14975, #4528, #12220, #1472, #4982, #819, #5074, #2211, #5215, #3445, #18135, #5486, #3819, #2226, #8116, #1827, #1097, #14091, #12645, #13424, #6926, #3247, #2156, #10911, #13243, #2026, #1316, #7945 ) ) ;
#15944 = ORIENTED_EDGE ( 'NONE', *, *, #13056, .F. ) ;
#15945 = CARTESIAN_POINT ( 'NONE',  ( 8.500000000000019540, 10.00000000000000000, 20.49999999999998934 ) ) ;
#15946 = CARTESIAN_POINT ( 'NONE',  ( 9.000000000000005329, 43.00000000000000000, 2.499999999999997335 ) ) ;
#15947 = CARTESIAN_POINT ( 'NONE',  ( -3.607379964056363075, 27.25319992234354771, -2.690724712371229899 ) ) ;
#15948 = CARTESIAN_POINT ( 'NONE',  ( 2.211161402132839182, 27.87819992234353705, -2.942372952327217739 ) ) ;
#15949 = CARTESIAN_POINT ( 'NONE',  ( 2.481649420246391902, 23.37819992234354771, 0.8687765177875720335 ) ) ;
#15950 = ORIENTED_EDGE ( 'NONE', *, *, #3325, .F. ) ;
#15951 = AXIS2_PLACEMENT_3D ( 'NONE', #8921, #316, #6051 ) ;
#15952 = CARTESIAN_POINT ( 'NONE',  ( -2.829195390882724315, 36.62819992234354771, 3.793023760679264722 ) ) ;
#15953 = VECTOR ( 'NONE', #2882, 1000.000000000000000 ) ;
#15954 = AXIS2_PLACEMENT_3D ( 'NONE', #8191, #13854, #1161 ) ;
#15955 = CARTESIAN_POINT ( 'NONE',  ( 2.000000000000004441, -18.90635161462267178, -8.759065166385774148 ) ) ;
#15956 = ORIENTED_EDGE ( 'NONE', *, *, #3400, .T. ) ;
#15957 = DIRECTION ( 'NONE',  ( -1.000000000000000000, 0.000000000000000000, 4.336808689942021680E-16 ) ) ;
#15958 = CARTESIAN_POINT ( 'NONE',  ( -2.211161402132902243, 33.37180007765648071, -2.942372952327172886 ) ) ;
#15959 = ADVANCED_FACE ( 'NONE', ( #4497 ), #17320, .T. ) ;
#15960 = CARTESIAN_POINT ( 'NONE',  ( -9.175662590029975973, -10.00000000000000000, -2.949107115053327011 ) ) ;
#15961 = CARTESIAN_POINT ( 'NONE',  ( 4.243569643750000786, -21.41596351010179333, -6.303685531992786473 ) ) ;
#15962 = CARTESIAN_POINT ( 'NONE',  ( -0.05938372350928957516, 28.62180007765647005, -4.731580009072201776 ) ) ;
#15963 = ADVANCED_FACE ( 'NONE', ( #14523 ), #11434, .F. ) ;
#15964 = CIRCLE ( 'NONE', #7349, 0.9999999999999991118 ) ;
#15965 = CARTESIAN_POINT ( 'NONE',  ( 4.243569643750000786, -27.09437022997710187, -14.41329077045383578 ) ) ;
#15966 = VERTEX_POINT ( 'NONE', #17126 ) ;
#15967 = CONICAL_SURFACE ( 'NONE', #7306, 3.309499999999999886, 0.7853981633974613796 ) ;
#15968 = CARTESIAN_POINT ( 'NONE',  ( -3.481649420246369697, 32.87180007765645939, 1.193696214020542490 ) ) ;
#15969 = CARTESIAN_POINT ( 'NONE',  ( 8.673617379884035472E-16, 0.000000000000000000, 0.000000000000000000 ) ) ;
#15970 = CARTESIAN_POINT ( 'NONE',  ( 3.579096709490575479E-14, -25.70887743576973605, -5.460814815566567226 ) ) ;
#15971 = DIRECTION ( 'NONE',  ( 0.000000000000000000, 0.000000000000000000, 1.000000000000000000 ) ) ;
#15972 = VERTEX_POINT ( 'NONE', #11717 ) ;
#15973 = CARTESIAN_POINT ( 'NONE',  ( 3.518350579753605434, 28.12819992234354416, -1.080741659609877114 ) ) ;
#15974 = CARTESIAN_POINT ( 'NONE',  ( 0.000000000000000000, 1.759474945355387954, 3.047499999999997211 ) ) ;
#15975 = CARTESIAN_POINT ( 'NONE',  ( -4.243569643750005227, -23.01423416803636002, -4.314762474715088558 ) ) ;
#15976 = CARTESIAN_POINT ( 'NONE',  ( 0.8262555684461332373, 24.74680007765647716, 2.360188852285403982 ) ) ;
#15977 = CARTESIAN_POINT ( 'NONE',  ( 2.211161402132839626, 32.87819992234354771, -2.942372952327218183 ) ) ;
#15978 = CARTESIAN_POINT ( 'NONE',  ( 8.000000000000005329, 16.59999999999999787, 2.499999999999997780 ) ) ;
#15979 = CARTESIAN_POINT ( 'NONE',  ( -2.000000000000005773, -29.35662728657488429, -11.60465181595445650 ) ) ;
#15980 = CONICAL_SURFACE ( 'NONE', #8539, 2.000000000000001776, 1.029744260000000189 ) ;
#15981 = CARTESIAN_POINT ( 'NONE',  ( 4.243569643750000786, -22.48066477007841613, -7.824236514204232940 ) ) ;
#15982 = VECTOR ( 'NONE', #6110, 1000.000000000000000 ) ;
#15983 = CARTESIAN_POINT ( 'NONE',  ( -7.506644857339464849, -12.68590315496589938, 7.157248747909027209 ) ) ;
#15984 = EDGE_CURVE ( 'NONE', #12418, #11008, #4584, .T. ) ;
#15985 = FACE_OUTER_BOUND ( 'NONE', #10540, .T. ) ;
#15986 = DIRECTION ( 'NONE',  ( -1.000000000000000000, -0.000000000000000000, -0.000000000000000000 ) ) ;
#15987 = VECTOR ( 'NONE', #15265, 1000.000000000000000 ) ;
#15988 = DIRECTION ( 'NONE',  ( -0.000000000000000000, -1.000000000000000000, -0.000000000000000000 ) ) ;
#15989 = VERTEX_POINT ( 'NONE', #12923 ) ;
#15990 = VERTEX_POINT ( 'NONE', #17222 ) ;
#15991 = CARTESIAN_POINT ( 'NONE',  ( 1.071796769724490339, -22.32902788685678885, -14.58146378416713773 ) ) ;
#15992 =( LENGTH_UNIT ( ) NAMED_UNIT ( * ) SI_UNIT ( .MILLI., .METRE. ) );
#15993 = ORIENTED_EDGE ( 'NONE', *, *, #1293, .T. ) ;
#15994 = VECTOR ( 'NONE', #542, 1000.000000000000000 ) ;
#15995 = CARTESIAN_POINT ( 'NONE',  ( 2.055738996568281518, 25.50319992234354416, -1.423772053676066518 ) ) ;
#15996 = CARTESIAN_POINT ( 'NONE',  ( 4.243569643750003451, -23.25915147027346563, -13.20752085500445894 ) ) ;
#15997 = CARTESIAN_POINT ( 'NONE',  ( -2.115076519116362519, 17.62180007765647716, 3.012182706137107147 ) ) ;
#15998 = CYLINDRICAL_SURFACE ( 'NONE', #1910, 0.9999999999999991118 ) ;
#15999 = DIRECTION ( 'NONE',  ( 1.000000000000000000, 0.000000000000000000, 0.000000000000000000 ) ) ;
#16000 = ORIENTED_EDGE ( 'NONE', *, *, #12603, .T. ) ;
#16001 = CARTESIAN_POINT ( 'NONE',  ( -1.734723475976807094E-15, 29.79999999999999716, -2.500000000000000000 ) ) ;
#16002 = CARTESIAN_POINT ( 'NONE',  ( 4.243569643749996345, -28.12264930428783671, -11.61033536916394304 ) ) ;
#16003 = AXIS2_PLACEMENT_3D ( 'NONE', #981, #10978, #18052 ) ;
#16004 = CARTESIAN_POINT ( 'NONE',  ( -2.000000000000005773, -27.87249825822150839, -9.485095902363450904 ) ) ;
#16005 = CARTESIAN_POINT ( 'NONE',  ( -4.243569643750000786, -23.60989337914451625, -9.436942101398194893 ) ) ;
#16006 = CARTESIAN_POINT ( 'NONE',  ( 8.500000000000001776, 10.00000000000000000, -18.34999999999999787 ) ) ;
#16007 = CARTESIAN_POINT ( 'NONE',  ( 3.885274725274725949, -4.336808689942017736E-16, 0.000000000000000000 ) ) ;
#16008 = DIRECTION ( 'NONE',  ( -1.000000000000000000, -0.000000000000000000, -0.000000000000000000 ) ) ;
#16009 = CARTESIAN_POINT ( 'NONE',  ( 4.243569643750003451, -21.96860448848362779, -11.36442875535422026 ) ) ;
#16010 = DIRECTION ( 'NONE',  ( -0.000000000000000000, -1.000000000000000000, -0.000000000000000000 ) ) ;
#16011 = DIRECTION ( 'NONE',  ( 0.000000000000000000, -1.000000000000000000, 0.000000000000000000 ) ) ;
#16012 = CARTESIAN_POINT ( 'NONE',  ( -0.05938372350926768989, 18.62180007765648071, -2.628655560595669183 ) ) ;
#16013 = CARTESIAN_POINT ( 'NONE',  ( 8.499999999999994671, 10.00000000000000000, 18.34999999999999787 ) ) ;
#16014 = CARTESIAN_POINT ( 'NONE',  ( -3.481649420246370141, 22.87180007765647716, 1.193696214020542268 ) ) ;
#16015 = CARTESIAN_POINT ( 'NONE',  ( 1.533898589781675205E-14, -26.99942441755958811, -7.303906915216807683 ) ) ;
#16016 = EDGE_CURVE ( 'NONE', #14161, #16574, #4744, .T. ) ;
#16017 = PRESENTATION_STYLE_ASSIGNMENT (( #10435 ) ) ;
#16018 = CARTESIAN_POINT ( 'NONE',  ( 4.000000000000003553, -24.06801372906273428, -14.11752367306045208 ) ) ;
#16019 = DIRECTION ( 'NONE',  ( 8.673617379884034239E-17, 0.000000000000000000, 1.000000000000000000 ) ) ;
#16020 = EDGE_CURVE ( 'NONE', #13486, #4985, #1491, .T. ) ;
#16021 = CARTESIAN_POINT ( 'NONE',  ( -1.135272562821019626, 19.00319992234354771, 3.311245368580577164 ) ) ;
#16022 = ORIENTED_EDGE ( 'NONE', *, *, #3092, .T. ) ;
#16023 = CARTESIAN_POINT ( 'NONE',  ( -4.243569643749998122, -21.39861290485976753, -10.55039641134203521 ) ) ;
#16024 = ADVANCED_FACE ( 'NONE', ( #17038 ), #13618, .T. ) ;
#16025 = CARTESIAN_POINT ( 'NONE',  ( -4.481649420246366589, 40.37180007765647360, 1.518615910253458878 ) ) ;
#16026 = ORIENTED_EDGE ( 'NONE', *, *, #8982, .T. ) ;
#16027 = EDGE_CURVE ( 'NONE', #17274, #5475, #7389, .T. ) ;
#16028 = DIRECTION ( 'NONE',  ( -3.469446951953613696E-16, -0.000000000000000000, -1.000000000000000000 ) ) ;
#16029 = DIRECTION ( 'NONE',  ( 0.000000000000000000, 0.000000000000000000, -1.000000000000000000 ) ) ;
#16030 = CARTESIAN_POINT ( 'NONE',  ( 4.243569643749996345, -27.09021171885596146, -10.13586168944375210 ) ) ;
#16031 = CYLINDRICAL_SURFACE ( 'NONE', #6980, 4.000000000000000000 ) ;
#16032 = AXIS2_PLACEMENT_3D ( 'NONE', #17415, #16010, #1926 ) ;
#16033 = CARTESIAN_POINT ( 'NONE',  ( 4.243569643750003451, -19.41977419944868544, -7.724321858545000197 ) ) ;
#16034 = ADVANCED_FACE ( 'NONE', ( #10328 ), #5883, .T. ) ;
#16035 = ORIENTED_EDGE ( 'NONE', *, *, #11981, .F. ) ;
#16036 = CARTESIAN_POINT ( 'NONE',  ( 3.064181913176683203, -21.66367673124435100, -2.174801284911689336 ) ) ;
#16037 = CYLINDRICAL_SURFACE ( 'NONE', #7778, 7.000000000000000000 ) ;
#16038 = CARTESIAN_POINT ( 'NONE',  ( 4.000000000000003553, -23.29368553998882518, -13.01166841327030710 ) ) ;
#16039 = VERTEX_POINT ( 'NONE', #4308 ) ;
#16040 = EDGE_LOOP ( 'NONE', ( #16296, #12037, #2246, #16344 ) ) ;
#16041 = DIRECTION ( 'NONE',  ( -0.000000000000000000, -0.5735764363510414965, -0.8191520442889950182 ) ) ;
#16042 = PRODUCT_DEFINITION ( 'UNKNOWN', '', #9239, #6491 ) ;
#16043 = DIRECTION ( 'NONE',  ( 0.000000000000000000, -1.000000000000000000, 0.000000000000000000 ) ) ;
#16044 = APPLICATION_PROTOCOL_DEFINITION ( 'draft international standard', 'automotive_design', 1998, #4162 ) ;
#16045 = CARTESIAN_POINT ( 'NONE',  ( 4.499999999999999112, 28.25319992234354416, 0.05647727720528474687 ) ) ;
#16046 = CARTESIAN_POINT ( 'NONE',  ( 2.864755990943222308, 38.00319992234354061, -2.011557305968548093 ) ) ;
#16047 = CARTESIAN_POINT ( 'NONE',  ( -0.8262555684460826111, 16.50319992234354416, 2.360188852285421302 ) ) ;
#16048 = EDGE_LOOP ( 'NONE', ( #4043, #16622, #14833 ) ) ;
#16049 = AXIS2_PLACEMENT_3D ( 'NONE', #6357, #10612, #14987 ) ;
#16050 = CARTESIAN_POINT ( 'NONE',  ( -0.05938372350928957516, 16.12180007765647716, -4.731580009072201776 ) ) ;
#16051 = CARTESIAN_POINT ( 'NONE',  ( -4.000000000000000888, -21.91605046519287825, -7.017883720103874623 ) ) ;
#16052 = VERTEX_POINT ( 'NONE', #9956 ) ;
#16053 = DIRECTION ( 'NONE',  ( -0.000000000000000000, -0.5735764363510414965, -0.8191520442889950182 ) ) ;
#16054 = CARTESIAN_POINT ( 'NONE',  ( 2.798362969681366330, 31.49680007765647716, -2.102939460078824929 ) ) ;
#16055 = DIRECTION ( 'NONE',  ( 1.000000000000000000, 0.000000000000000000, 0.000000000000000000 ) ) ;
#16056 = CARTESIAN_POINT ( 'NONE',  ( -2.121784821875005722, -24.51241577880647782, -4.318642500053448963 ) ) ;
#16057 = CARTESIAN_POINT ( 'NONE',  ( -3.673772985318219053, 33.24680007765647360, -2.599342558260952174 ) ) ;
#16058 = MECHANICAL_DESIGN_GEOMETRIC_PRESENTATION_REPRESENTATION (  '', ( #5679 ), #9825 ) ;
#16059 = DIRECTION ( 'NONE',  ( 0.000000000000000000, 0.5150380737757255245, 0.8571673013836856869 ) ) ;
#16060 = ORIENTED_EDGE ( 'NONE', *, *, #15325, .F. ) ;
#16061 = CARTESIAN_POINT ( 'NONE',  ( 2.211161402132902243, 32.12180007765647360, 2.942372952327172442 ) ) ;
#16062 = CARTESIAN_POINT ( 'NONE',  ( -1.999999999999996225, -17.05656760739055500, -6.117299823553768334 ) ) ;
#16063 = CARTESIAN_POINT ( 'NONE',  ( 4.000000000000000000, 1.759474945355381514, -3.047500000000001652 ) ) ;
#16064 = CARTESIAN_POINT ( 'NONE',  ( -15.00000000000000178, 13.00000000000000178, -25.00000000000000355 ) ) ;
#16065 = VERTEX_POINT ( 'NONE', #15722 ) ;
#16066 = CARTESIAN_POINT ( 'NONE',  ( -3.518350579753605434, 26.87819992234354416, 1.080741659609877781 ) ) ;
#16067 = DIRECTION ( 'NONE',  ( -1.000000000000000000, -0.000000000000000000, -0.000000000000000000 ) ) ;
#16068 = CARTESIAN_POINT ( 'NONE',  ( 4.243569643750003451, -19.38751052490393434, -7.678244556053742897 ) ) ;
#16069 = CARTESIAN_POINT ( 'NONE',  ( -2.055738996568313048, 18.24680007765647716, -1.423772053676023441 ) ) ;
#16070 = AXIS2_PLACEMENT_3D ( 'NONE', #107, #15870, #3167 ) ;
#16071 = CARTESIAN_POINT ( 'NONE',  ( 4.518350579753602325, 18.12819992234354416, -1.405661355842793725 ) ) ;
#16072 = VECTOR ( 'NONE', #15428, 1000.000000000000000 ) ;
#16073 = CARTESIAN_POINT ( 'NONE',  ( -2.121784821875005722, -29.70686738051060161, -11.73708820114566009 ) ) ;
#16074 = CARTESIAN_POINT ( 'NONE',  ( -4.000000000000000888, -26.04580080692037569, -12.91577843898463840 ) ) ;
#16075 = AXIS2_PLACEMENT_3D ( 'NONE', #1830, #10055, #10337 ) ;
#16076 = CARTESIAN_POINT ( 'NONE',  ( -4.243569643750005227, -23.56271663529704696, -5.098076617066438665 ) ) ;
#16077 = LINE ( 'NONE', #13089, #12461 ) ;
#16078 = CARTESIAN_POINT ( 'NONE',  ( -3.412954772041501439, -15.19080604886724473, -9.070274817126582789 ) ) ;
#16079 = AXIS2_PLACEMENT_3D ( 'NONE', #4238, #1369, #14432 ) ;
#16080 = CARTESIAN_POINT ( 'NONE',  ( 3.999999999999996447, -22.15159911833919182, -3.327964152506997397 ) ) ;
#16081=STYLED_ITEM('',(#18396),#2004);
#16082 = CARTESIAN_POINT ( 'NONE',  ( 1.533898589781675205E-14, -27.96733465319702105, -8.686225988947720467 ) ) ;
#16083 = ORIENTED_EDGE ( 'NONE', *, *, #7600, .F. ) ;
#16084 = EDGE_LOOP ( 'NONE', ( #11515, #8579, #6058, #11820 ) ) ;
#16085 = CARTESIAN_POINT ( 'NONE',  ( -1.071796769724477238, -22.88120077655093354, -1.422474030991951688 ) ) ;
#16086 = CARTESIAN_POINT ( 'NONE',  ( 3.999999999999996447, -27.57189644185653066, -11.06895097103799941 ) ) ;
#16087 = CYLINDRICAL_SURFACE ( 'NONE', #9993, 0.9999999999999991118 ) ;
#16088 = ORIENTED_EDGE ( 'NONE', *, *, #13222, .F. ) ;
#16089 = CARTESIAN_POINT ( 'NONE',  ( 2.518350579753611207, 25.62819992234354416, -0.7558219633769606149 ) ) ;
#16090 = DIRECTION ( 'NONE',  ( 0.000000000000000000, 0.000000000000000000, 1.000000000000000000 ) ) ;
#16091 = COLOUR_RGB ( '',0.8941176470588234615, 0.8941176470588234615, 0.8941176470588234615 ) ;
#16092 = CARTESIAN_POINT ( 'NONE',  ( -4.243569643750005227, -27.14398450976385746, -10.21265719359585233 ) ) ;
#16093 = CARTESIAN_POINT ( 'NONE',  ( -3.518350579753630747, 20.62180007765646650, -1.080741659609802729 ) ) ;
#16094 = VECTOR ( 'NONE', #2514, 1000.000000000000000 ) ;
#16095 = FACE_OUTER_BOUND ( 'NONE', #14317, .T. ) ;
#16096 = EDGE_CURVE ( 'NONE', #14197, #5921, #427, .T. ) ;
#16097 = CARTESIAN_POINT ( 'NONE',  ( 5.002737418183710538, -14.83391033323059993, -6.661572473864424637 ) ) ;
#16098 = CIRCLE ( 'NONE', #16386, 7.500000000000000888 ) ;
#16099 = CARTESIAN_POINT ( 'NONE',  ( 2.121784821874994176, -28.63141156235240459, -10.20117811810379216 ) ) ;
#16100 =( BOUNDED_CURVE ( )  B_SPLINE_CURVE ( 2, ( #17562, #10482, #10193, #14487, #14579, #15873, #12982, #3077, #1883 ),
 .UNSPECIFIED., .F., .T. ) 
 B_SPLINE_CURVE_WITH_KNOTS ( ( 3, 2, 2, 2, 3 ),
 ( 0.3017241379310345306, 0.3045977011494253039, 0.3103448275862069061, 0.3160919540229885083, 0.3189655172413793371 ),
 .UNSPECIFIED. ) 
 CURVE ( )  GEOMETRIC_REPRESENTATION_ITEM ( )  RATIONAL_B_SPLINE_CURVE ( ( 0.9330127018922194093, 0.9330127018922200755, 1.000000000000000000, 0.8660254037844387076, 1.000000000000000000, 0.8660254037844387076, 1.000000000000000000, 0.9330127018922187432, 0.9330127018922194093 ) ) 
 REPRESENTATION_ITEM ( '' )  );
#16101 = CARTESIAN_POINT ( 'NONE',  ( -1.071796769724486564, -27.46264256119991742, -7.965450983743535218 ) ) ;
#16102 = CARTESIAN_POINT ( 'NONE',  ( 4.243569643750000786, -24.51327626639741553, -10.72710657115335842 ) ) ;
#16103 = LINE ( 'NONE', #2011, #13017 ) ;
#16104 = DIRECTION ( 'NONE',  ( -0.000000000000000000, 1.000000000000000000, -0.000000000000000000 ) ) ;
#16105 = CARTESIAN_POINT ( 'NONE',  ( 4.243569643750003451, -20.67805750669378284, -9.521336655703981577 ) ) ;
#16106 = CARTESIAN_POINT ( 'NONE',  ( 0.000000000000000000, 0.000000000000000000, 0.000000000000000000 ) ) ;
#16107 = CIRCLE ( 'NONE', #100, 10.00000000000000178 ) ;
#16108 = DIRECTION ( 'NONE',  ( 1.000000000000000000, 0.000000000000000000, -4.336808689942021680E-16 ) ) ;
#16109 = CARTESIAN_POINT ( 'NONE',  ( 1.593127413382998903, 27.12180007765647716, 2.091722143975139669 ) ) ;
#16110 = VERTEX_POINT ( 'NONE', #2930 ) ;
#16111 = CARTESIAN_POINT ( 'NONE',  ( 3.518350579753631191, 26.87180007765647716, 1.080741659609802729 ) ) ;
#16112 = CYLINDRICAL_SURFACE ( 'NONE', #6873, 0.9999999999999991118 ) ;
#16113 = CARTESIAN_POINT ( 'NONE',  ( 1.999999999999994449, -28.08758942185315988, -9.792277918971819872 ) ) ;
#16114 = DIRECTION ( 'NONE',  ( -1.000000000000000000, -0.000000000000000000, -0.000000000000000000 ) ) ;
#16115 = CARTESIAN_POINT ( 'NONE',  ( 2.211161402132839626, 20.37819992234354416, -2.942372952327218183 ) ) ;
#16116 = ORIENTED_EDGE ( 'NONE', *, *, #5520, .F. ) ;
#16117 = CARTESIAN_POINT ( 'NONE',  ( 4.243569643750000786, -22.73877416643638227, -8.192854934134281564 ) ) ;
#16118 = CARTESIAN_POINT ( 'NONE',  ( 2.829195390882805583, 39.62180007765647360, 3.793023760679204770 ) ) ;
#16119 = ORIENTED_EDGE ( 'NONE', *, *, #17463, .F. ) ;
#16120 = PRODUCT_DEFINITION_SHAPE ( 'NONE', 'NONE',  #11945 ) ;
#16121 = DIRECTION ( 'NONE',  ( -0.000000000000000000, 0.000000000000000000, 1.000000000000000000 ) ) ;
#16122 = FACE_OUTER_BOUND ( 'NONE', #12955, .T. ) ;
#16123 = EDGE_CURVE ( 'NONE', #13373, #8755, #12427, .T. ) ;
#16124 = CARTESIAN_POINT ( 'NONE',  ( 4.243569643749996345, -28.12264930428783671, -11.61033536916394304 ) ) ;
#16125 = DIRECTION ( 'NONE',  ( -0.000000000000000000, -0.000000000000000000, -1.000000000000000000 ) ) ;
#16126 = CARTESIAN_POINT ( 'NONE',  ( 7.191589934391299899, -10.00000000000000000, 14.52136967842654158 ) ) ;
#16127 = EDGE_CURVE ( 'NONE', #1346, #11263, #9476, .T. ) ;
#16128 = AXIS2_PLACEMENT_3D ( 'NONE', #18162, #10719, #13496 ) ;
#16129 = DIRECTION ( 'NONE',  ( 0.000000000000000000, 0.000000000000000000, -1.000000000000000000 ) ) ;
#16130 = CARTESIAN_POINT ( 'NONE',  ( -2.121784821875005722, -22.99602307520341427, -2.153009282964420290 ) ) ;
#16131 = ORIENTED_EDGE ( 'NONE', *, *, #2006, .F. ) ;
#16132 = DIRECTION ( 'NONE',  ( 6.162975822039154730E-33, -0.5735764363510414965, -0.8191520442889950182 ) ) ;
#16133 = CARTESIAN_POINT ( 'NONE',  ( -4.000000000000000888, -23.52923419313512454, -9.321748845673438311 ) ) ;
#16134 = PLANE ( 'NONE',  #11456 ) ;
#16135 = EDGE_LOOP ( 'NONE', ( #12125, #15532, #1388, #12286 ) ) ;
#16136 = VERTEX_POINT ( 'NONE', #14238 ) ;
#16137 = CARTESIAN_POINT ( 'NONE',  ( 2.000000000000004441, -21.29386353163882717, -12.16878555174548104 ) ) ;
#16138 = LINE ( 'NONE', #15849, #1270 ) ;
#16139 =( LENGTH_UNIT ( ) NAMED_UNIT ( * ) SI_UNIT ( .MILLI., .METRE. ) );
#16140 = CARTESIAN_POINT ( 'NONE',  ( 2.829195390882724759, 25.37819992234354416, -3.793023760679264278 ) ) ;
#16141 = CARTESIAN_POINT ( 'NONE',  ( -8.500000000000005329, 10.00000000000000000, -18.35000000000000142 ) ) ;
#16142 = CARTESIAN_POINT ( 'NONE',  ( -0.7188294034286550893, 20.00319992234354771, -2.395093729190349130 ) ) ;
#16143 = ORIENTED_EDGE ( 'NONE', *, *, #14601, .F. ) ;
#16144 = CARTESIAN_POINT ( 'NONE',  ( -0.05938372350928957516, 21.12180007765647360, -4.731580009072201776 ) ) ;
#16145 = CARTESIAN_POINT ( 'NONE',  ( -1.999999999999996225, -19.63766157097024490, -9.803484022854247470 ) ) ;
#16146 = EDGE_LOOP ( 'NONE', ( #14152, #10406, #5167, #7715 ) ) ;
#16147 = CARTESIAN_POINT ( 'NONE',  ( -2.864755990943265829, 35.74680007765648071, -2.011557305968488141 ) ) ;
#16148 = CARTESIAN_POINT ( 'NONE',  ( -1.661723472263481630E-14, -20.51073541163217584, -11.98467301000088803 ) ) ;
#16149 = EDGE_CURVE ( 'NONE', #7195, #16065, #6112, .T. ) ;
#16150 = CARTESIAN_POINT ( 'NONE',  ( 2.121784821875004390, -17.84631068140748766, -7.612928127393706390 ) ) ;
#16151 = ADVANCED_FACE ( 'NONE', ( #7266 ), #235, .F. ) ;
#16152 = CARTESIAN_POINT ( 'NONE',  ( 4.243569643750000786, -24.28743054458419692, -10.40456545371456620 ) ) ;
#16153 = DIRECTION ( 'NONE',  ( 0.000000000000000000, 0.000000000000000000, 1.000000000000000000 ) ) ;
#16154 = ORIENTED_EDGE ( 'NONE', *, *, #11437, .F. ) ;
#16155 = CARTESIAN_POINT ( 'NONE',  ( 1.801903668194569486, -10.00000000000000178, 23.81845480839541196 ) ) ;
#16156 = LINE ( 'NONE', #7515, #9822 ) ;
#16157 = ORIENTED_EDGE ( 'NONE', *, *, #12726, .T. ) ;
#16158 = CARTESIAN_POINT ( 'NONE',  ( -1.135272562821019626, 24.00319992234354416, 3.311245368580577164 ) ) ;
#16159 = DIRECTION ( 'NONE',  ( 0.000000000000000000, 0.000000000000000000, -1.000000000000000000 ) ) ;
#16160 = CARTESIAN_POINT ( 'NONE',  ( 4.730628863548789710E-15, -18.11187661241681823, -10.12794063824400581 ) ) ;
#16161 = CARTESIAN_POINT ( 'NONE',  ( 0.7188294034286049072, 21.24680007765648426, -2.395093729190366005 ) ) ;
#16162 = CARTESIAN_POINT ( 'NONE',  ( 3.607379964056363075, 21.00319992234354416, 2.690724712371229010 ) ) ;
#16163 = CARTESIAN_POINT ( 'NONE',  ( 12.00000000000000178, 48.00000000000000000, 15.00000000000000000 ) ) ;
#16164 = CARTESIAN_POINT ( 'NONE',  ( -1.999999999999996225, -24.02552130905571204, -16.06999716166505721 ) ) ;
#16165 = CARTESIAN_POINT ( 'NONE',  ( 4.243569643750003451, -19.41977419944868544, -7.724321858545000197 ) ) ;
#16166 = CARTESIAN_POINT ( 'NONE',  ( 0.000000000000000000, 5.977523610840987267, 32.81826849749789687 ) ) ;
#16167 = DIRECTION ( 'NONE',  ( -1.000000000000000000, 0.000000000000000000, 4.336808689942021680E-16 ) ) ;
#16168 = PLANE ( 'NONE',  #17200 ) ;
#16169 = CARTESIAN_POINT ( 'NONE',  ( -5.577813053751546416E-15, -29.06429958842333505, -10.25285427465718691 ) ) ;
#16170 = VERTEX_POINT ( 'NONE', #16186 ) ;
#16171 = EDGE_LOOP ( 'NONE', ( #10661, #16711, #17678, #5442 ) ) ;
#16172 = FILL_AREA_STYLE ('',( #597 ) ) ;
#16173 = CARTESIAN_POINT ( 'NONE',  ( -10.00000000000000000, 25.39999999999999503, 2.499999999999998224 ) ) ;
#16174 = EDGE_LOOP ( 'NONE', ( #14358, #9981, #11588, #12067 ) ) ;
#16175 = CARTESIAN_POINT ( 'NONE',  ( -0.8262555684460826111, 31.50319992234354416, 2.360188852285421302 ) ) ;
#16176 = CARTESIAN_POINT ( 'NONE',  ( 2.121784821874994176, -28.59914788780765704, -10.15510081561253664 ) ) ;
#16177 = CARTESIAN_POINT ( 'NONE',  ( 3.500000000000000444, 26.74680007765648071, -0.05647727720536935281 ) ) ;
#16178 = VECTOR ( 'NONE', #3973, 1000.000000000000000 ) ;
#16179 = CARTESIAN_POINT ( 'NONE',  ( -0.2979626678802195783, -10.00000000000000355, -4.943697222985274919 ) ) ;
#16180 = CARTESIAN_POINT ( 'NONE',  ( 2.121784821875004390, -23.04076228311161145, -15.03137382848591663 ) ) ;
#16181 = EDGE_CURVE ( 'NONE', #9997, #15303, #4, .T. ) ;
#16182 = EDGE_CURVE ( 'NONE', #218, #2069, #8003, .T. ) ;
#16183 = CARTESIAN_POINT ( 'NONE',  ( -4.243569643749998122, -22.65689621210486138, -12.34741120850101836 ) ) ;
#16184 = CARTESIAN_POINT ( 'NONE',  ( 3.375445829055900404, -25.20600189401019264, -15.83707978931157534 ) ) ;
#16185 = ADVANCED_FACE ( 'NONE', ( #10699 ), #3563, .T. ) ;
#16186 = CARTESIAN_POINT ( 'NONE',  ( -8.500000000000005329, 14.99364916731036956, -22.64999999999999147 ) ) ;
#16187 = EDGE_CURVE ( 'NONE', #3470, #13534, #10358, .T. ) ;
#16188 = CARTESIAN_POINT ( 'NONE',  ( 3.579096709490575479E-14, -23.64400226490599266, -2.511867456126184894 ) ) ;
#16189 = TOROIDAL_SURFACE ( 'NONE', #9663, 2.200000000000000178, 0.2000000000000000111 ) ;
#16190 = CARTESIAN_POINT ( 'NONE',  ( 4.243569643750000786, -23.22272928460757413, -8.884014471503119736 ) ) ;
#16191 = B_SPLINE_CURVE_WITH_KNOTS ( 'NONE', 3,
 ( #2748, #2833, #16941, #8380, #9861, #14042, #6983, #15808, #18335, #12644, #7350, #2919, #7166, #223 ),
 .UNSPECIFIED., .F., .F.,
 ( 4, 2, 2, 2, 2, 2, 4 ),
 ( 0.000000000000000000, 0.002373381915594256590, 0.004746763831188513180, 0.007120145746782769770, 0.009493527662377028095, 0.01424029149356554128, 0.01898705532475405272 ),
 .UNSPECIFIED. ) ;
#16192 = ORIENTED_EDGE ( 'NONE', *, *, #8774, .F. ) ;
#16193 = DIRECTION ( 'NONE',  ( 0.000000000000000000, 0.8191520442889952403, -0.5735764363510413855 ) ) ;
#16194 = CARTESIAN_POINT ( 'NONE',  ( 1.533898589781675205E-14, -27.70922525683905846, -8.317607569017670954 ) ) ;
#16195 = CARTESIAN_POINT ( 'NONE',  ( -1.989345975306426206, 32.74680007765648071, 1.515154207786343799 ) ) ;
#16196 = ORIENTED_EDGE ( 'NONE', *, *, #950, .F. ) ;
#16197 = CARTESIAN_POINT ( 'NONE',  ( -3.481649420246370141, 27.87180007765647716, 1.193696214020542268 ) ) ;
#16198 = CARTESIAN_POINT ( 'NONE',  ( -4.000000000000004441, -25.65758508623986245, -8.335031024230248775 ) ) ;
#16199 = DIRECTION ( 'NONE',  ( -0.8191520442889950182, -0.4698463103929522156, 0.3289899283371602867 ) ) ;
#16200 = CARTESIAN_POINT ( 'NONE',  ( 1.071796769724495224, -16.97325791313388521, -6.932631571625408995 ) ) ;
#16201 = CARTESIAN_POINT ( 'NONE',  ( -1.027846397803611866, 17.50319992234354416, -3.346150245485499219 ) ) ;
#16202 =( BOUNDED_CURVE ( )  B_SPLINE_CURVE ( 1, ( #8998, #10187 ),
 .UNSPECIFIED., .F., .T. ) 
 B_SPLINE_CURVE_WITH_KNOTS ( ( 2, 2 ),
 ( 0.000000000000000000, 1.000000000000000000 ),
 .UNSPECIFIED. ) 
 CURVE ( )  GEOMETRIC_REPRESENTATION_ITEM ( )  RATIONAL_B_SPLINE_CURVE ( ( 0.9401542295229485813, 0.9401542295229485813 ) ) 
 REPRESENTATION_ITEM ( '' )  );
#16203 = ORIENTED_EDGE ( 'NONE', *, *, #11573, .F. ) ;
#16204 = CARTESIAN_POINT ( 'NONE',  ( -4.243569643749998122, -21.14050350850180138, -10.18177799141198747 ) ) ;
#16205 = CARTESIAN_POINT ( 'NONE',  ( -0.05938372350927861171, 18.62180007765647005, -3.680117784833935701 ) ) ;
#16206 = VECTOR ( 'NONE', #979, 1000.000000000000000 ) ;
#16207 = ORIENTED_EDGE ( 'NONE', *, *, #5974, .T. ) ;
#16208 = DIRECTION ( 'NONE',  ( 1.000000000000000000, 0.000000000000000000, -0.000000000000000000 ) ) ;
#16209 = EDGE_CURVE ( 'NONE', #6738, #1326, #6255, .T. ) ;
#16210 = CARTESIAN_POINT ( 'NONE',  ( 2.121784821875004390, -23.04076228311161145, -15.03137382848591663 ) ) ;
#16211 = CARTESIAN_POINT ( 'NONE',  ( 4.299564228933482956E-15, -23.34993877156982833, -16.03947562923141135 ) ) ;
#16212 = CARTESIAN_POINT ( 'NONE',  ( 6.268704630795123300, -10.34422234558816633, 0.7521107233528409042 ) ) ;
#16213 = CARTESIAN_POINT ( 'NONE',  ( -1.071796769724496334, -21.78975569270318502, -13.81130327499520760 ) ) ;
#16214 = CARTESIAN_POINT ( 'NONE',  ( 4.243569643749996345, -22.44424258441252817, -3.500730130702893739 ) ) ;
#16215 = VERTEX_POINT ( 'NONE', #9035 ) ;
#16216 = CARTESIAN_POINT ( 'NONE',  ( 3.999999999999996447, -25.05532982807127951, -7.474921377726801097 ) ) ;
#16217 = CARTESIAN_POINT ( 'NONE',  ( 4.000000000000003553, -21.48691976548304794, -10.43133947375997295 ) ) ;
#16218 = VERTEX_POINT ( 'NONE', #17688 ) ;
#16219 = CONICAL_SURFACE ( 'NONE', #12058, 3.309499999999999886, 0.7853981633974613796 ) ;
#16220 = ORIENTED_EDGE ( 'NONE', *, *, #17754, .T. ) ;
#16221 = CARTESIAN_POINT ( 'NONE',  ( -3.706921591972381904E-14, -18.18775084441045209, -8.667107230630458403 ) ) ;
#16222 = CARTESIAN_POINT ( 'NONE',  ( 0.000000000000000000, 5.977523610840987267, 32.81826849749789687 ) ) ;
#16223 = SURFACE_STYLE_USAGE ( .BOTH. , #10735 ) ;
#16224 = CARTESIAN_POINT ( 'NONE',  ( 2.829195390882724759, 27.87819992234354416, -3.793023760679264278 ) ) ;
#16225 = CARTESIAN_POINT ( 'NONE',  ( -2.864755990943222308, 34.25319992234354771, 2.011557305968548093 ) ) ;
#16226 = CARTESIAN_POINT ( 'NONE',  ( -1.989345975306457071, 19.75319992234354771, -1.515154207786300944 ) ) ;
#16227 = ORIENTED_EDGE ( 'NONE', *, *, #10346, .T. ) ;
#16228 = CARTESIAN_POINT ( 'NONE',  ( -4.499999999999999112, 20.49680007765647716, 0.05647727720537927543 ) ) ;
#16229 = CARTESIAN_POINT ( 'NONE',  ( -4.000000000000000888, -22.43226925790881765, -7.755120559963970983 ) ) ;
#16230 = CLOSED_SHELL ( 'NONE', ( #2861, #8722, #5852, #33, #957, #12086, #11518, #6377, #2865, #13156 ) ) ;
#16231 = EDGE_LOOP ( 'NONE', ( #16818, #16246, #6456 ) ) ;
#16232 = EDGE_CURVE ( 'NONE', #11085, #17274, #601, .T. ) ;
#16233 = AXIS2_PLACEMENT_3D ( 'NONE', #12639, #11247, #17025 ) ;
#16234 = CARTESIAN_POINT ( 'NONE',  ( 4.898587196589413815E-16, 2.700915433685006750, 35.11257424290206330 ) ) ;
#16235 = CIRCLE ( 'NONE', #231, 10.00000000000000178 ) ;
#16236 = CARTESIAN_POINT ( 'NONE',  ( -3.481649420246369697, 37.87180007765648071, 1.193696214020542490 ) ) ;
#16237 = DIRECTION ( 'NONE',  ( 0.000000000000000000, 0.000000000000000000, -1.000000000000000000 ) ) ;
#16238 = CARTESIAN_POINT ( 'NONE',  ( -4.243569643749998122, -18.52714587037736749, -6.449516489620252813 ) ) ;
#16239 = CARTESIAN_POINT ( 'NONE',  ( 4.243569643750000786, -23.77121175186825752, -9.667328613854474284 ) ) ;
#16240 = PLANE ( 'NONE',  #12386 ) ;
#16241 = ORIENTED_EDGE ( 'NONE', *, *, #7835, .F. ) ;
#16242 = CARTESIAN_POINT ( 'NONE',  ( -1.522508701837280043, -9.999999999999175770, 22.87631747054243903 ) ) ;
#16243 = DIRECTION ( 'NONE',  ( 0.000000000000000000, 0.000000000000000000, 1.000000000000000000 ) ) ;
#16244 = DIRECTION ( 'NONE',  ( -1.000000000000000000, 0.000000000000000000, 4.336808689942021680E-16 ) ) ;
#16245 = CARTESIAN_POINT ( 'NONE',  ( 4.243569643750000786, -26.61041511180591357, -13.72213123308499760 ) ) ;
#16246 = ORIENTED_EDGE ( 'NONE', *, *, #17924, .F. ) ;
#16247 = AXIS2_PLACEMENT_3D ( 'NONE', #13187, #5866, #14402 ) ;
#16248 = CARTESIAN_POINT ( 'NONE',  ( 2.115076519116426024, 31.12819992234354061, 3.012182706137062294 ) ) ;
#16249 = CARTESIAN_POINT ( 'NONE',  ( 2.798362969681409851, 16.00319992234354416, 2.102939460078764977 ) ) ;
#16250 = AXIS2_PLACEMENT_3D ( 'NONE', #2721, #8435, #18302 ) ;
#16251 = CARTESIAN_POINT ( 'NONE',  ( -5.330712181944245322E-15, -25.23626920050269362, -3.216667265601666603 ) ) ;
#16252 = CARTESIAN_POINT ( 'NONE',  ( -1.593127413382998459, 20.87180007765648426, -2.091722143975139669 ) ) ;
#16253 = ADVANCED_FACE ( 'NONE', ( #3481 ), #4954, .T. ) ;
#16254 = CARTESIAN_POINT ( 'NONE',  ( -3.607379964056363075, 14.75319992234354416, -2.690724712371229899 ) ) ;
#16255 = CARTESIAN_POINT ( 'NONE',  ( 4.243569643750000786, -26.86852450816387972, -14.09074965301504534 ) ) ;
#16256 = ADVANCED_FACE ( 'NONE', ( #17784 ), #13917, .T. ) ;
#16257 = CARTESIAN_POINT ( 'NONE',  ( 4.713407268011036227E-15, -22.32682692979000549, -15.65716912339195233 ) ) ;
#16258 = EDGE_CURVE ( 'NONE', #10807, #7842, #11793, .T. ) ;
#16259 = CARTESIAN_POINT ( 'NONE',  ( -4.243569643749997233, -19.07562833763805088, -7.232830631971606472 ) ) ;
#16260 = CARTESIAN_POINT ( 'NONE',  ( -2.864755990943265829, 15.74680007765647716, -2.011557305968488141 ) ) ;
#16261 = EDGE_CURVE ( 'NONE', #4334, #177, #17868, .T. ) ;
#16262 = VECTOR ( 'NONE', #1118, 1000.000000000000000 ) ;
#16263 = DIRECTION ( 'NONE',  ( -0.000000000000000000, -0.5735764363510414965, -0.8191520442889950182 ) ) ;
#16264 = CARTESIAN_POINT ( 'NONE',  ( -1.734723475976807094E-15, 25.39999999999999503, -2.500000000000000000 ) ) ;
#16265 = DIRECTION ( 'NONE',  ( -0.000000000000000000, -1.000000000000000000, -0.000000000000000000 ) ) ;
#16266 = ORIENTED_EDGE ( 'NONE', *, *, #8614, .T. ) ;
#16267 = VERTEX_POINT ( 'NONE', #9127 ) ;
#16268 = LINE ( 'NONE', #6423, #3521 ) ;
#16269 = LINE ( 'NONE', #13098, #952 ) ;
#16270 = CARTESIAN_POINT ( 'NONE',  ( 4.000000000000000888, -25.91674610874139972, -12.73146922901961098 ) ) ;
#16271 = ORIENTED_EDGE ( 'NONE', *, *, #16209, .T. ) ;
#16272 = CARTESIAN_POINT ( 'NONE',  ( 0.05938372350921204690, 25.12819992234354416, -2.628655560595669183 ) ) ;
#16273 = CARTESIAN_POINT ( 'NONE',  ( 2.121784821874994176, -29.11536668052359289, -10.89233765547263211 ) ) ;
#16274 = CARTESIAN_POINT ( 'NONE',  ( 2.211161402132902243, 19.62180007765647360, 2.942372952327172442 ) ) ;
#16275 = CIRCLE ( 'NONE', #17776, 0.9999999999999991118 ) ;
#16276 = AXIS2_PLACEMENT_3D ( 'NONE', #15005, #538, #6457 ) ;
#16277 = CARTESIAN_POINT ( 'NONE',  ( 4.000000000000000000, 3.518949890710770134, -4.119968255444916849E-15 ) ) ;
#16278 = VECTOR ( 'NONE', #658, 1000.000000000000000 ) ;
#16279 = FACE_OUTER_BOUND ( 'NONE', #3050, .T. ) ;
#16280 = CARTESIAN_POINT ( 'NONE',  ( 2.121784821875004390, -22.26643409403770590, -13.92551856869577342 ) ) ;
#16281 = AXIS2_PLACEMENT_3D ( 'NONE', #3189, #17108, #15530 ) ;
#16282 = LINE ( 'NONE', #16560, #12032 ) ;
#16283 = VECTOR ( 'NONE', #75, 1000.000000000000000 ) ;
#16284 = DIRECTION ( 'NONE',  ( 0.000000000000000000, -1.000000000000000000, 0.000000000000000000 ) ) ;
#16285 = CARTESIAN_POINT ( 'NONE',  ( 8.673617379884035472E-15, 10.00000000000000000, 3.469446951953614189E-15 ) ) ;
#16286 = CARTESIAN_POINT ( 'NONE',  ( 4.243569643750003451, -21.45238569576768484, -10.62719191549412656 ) ) ;
#16287 = ORIENTED_EDGE ( 'NONE', *, *, #7189, .T. ) ;
#16288 = CARTESIAN_POINT ( 'NONE',  ( -1.734723475976807094E-15, 29.79999999999999716, -2.500000000000000000 ) ) ;
#16289 = DIRECTION ( 'NONE',  ( 1.028113302204111856E-14, -0.1129545544106654864, 0.9936001553129347741 ) ) ;
#16290 = CARTESIAN_POINT ( 'NONE',  ( -2.500000000000001332, 30.49680007765648071, 0.05647727720535858364 ) ) ;
#16291 = DIRECTION ( 'NONE',  ( -0.000000000000000000, -0.5735764363510414965, -0.8191520442889950182 ) ) ;
#16292 = CARTESIAN_POINT ( 'NONE',  ( -3.500000000000000444, 32.99680007765648071, 0.05647727720536892260 ) ) ;
#16293 = DIRECTION ( 'NONE',  ( -3.469446951953613696E-16, -0.000000000000000000, -1.000000000000000000 ) ) ;
#16294 = PRODUCT_CONTEXT ( 'NONE', #7947, 'mechanical' ) ;
#16295 = CARTESIAN_POINT ( 'NONE',  ( 4.000000000000003553, -18.38960700918742219, -6.007918434599401003 ) ) ;
#16296 = ORIENTED_EDGE ( 'NONE', *, *, #15819, .T. ) ;
#16297 = CARTESIAN_POINT ( 'NONE',  ( 4.243569643749997233, -24.25100835891830542, -6.081059070213227891 ) ) ;
#16298 = AXIS2_PLACEMENT_3D ( 'NONE', #8748, #334, #1726 ) ;
#16299 = CARTESIAN_POINT ( 'NONE',  ( -0.05938372350927861171, 16.12180007765647716, -3.680117784833935701 ) ) ;
#16300 = ORIENTED_EDGE ( 'NONE', *, *, #10214, .F. ) ;
#16301 = EDGE_CURVE ( 'NONE', #11633, #10059, #7913, .T. ) ;
#16302 = DIRECTION ( 'NONE',  ( 0.000000000000000000, 0.000000000000000000, 1.000000000000000000 ) ) ;
#16303 = DIRECTION ( 'NONE',  ( 0.000000000000000000, 0.000000000000000000, 1.000000000000000000 ) ) ;
#16304 = CARTESIAN_POINT ( 'NONE',  ( -3.537377991931545118, -25.46155756473516263, -15.53479600987054532 ) ) ;
#16305 = DIRECTION ( 'NONE',  ( 0.000000000000000000, -1.000000000000000000, 0.000000000000000000 ) ) ;
#16306 = CARTESIAN_POINT ( 'NONE',  ( 9.909030972036948270, -9.930865375757933933, 8.916665252758585680 ) ) ;
#16307 = DIRECTION ( 'NONE',  ( 0.000000000000000000, 0.000000000000000000, -1.000000000000000000 ) ) ;
#16308 = CARTESIAN_POINT ( 'NONE',  ( -5.330712181944245322E-15, -23.71987649689963362, -1.051034048512634156 ) ) ;
#16309 = ORIENTED_EDGE ( 'NONE', *, *, #7625, .F. ) ;
#16310 = DIRECTION ( 'NONE',  ( -1.000000000000000000, 0.000000000000000000, 4.336808689942021680E-16 ) ) ;
#16311 = CARTESIAN_POINT ( 'NONE',  ( 2.000000000000004441, -19.74520715349101607, -9.957075032165194628 ) ) ;
#16312 = AXIS2_PLACEMENT_3D ( 'NONE', #2999, #11604, #8724 ) ;
#16313 = ORIENTED_EDGE ( 'NONE', *, *, #18026, .F. ) ;
#16314 = ORIENTED_EDGE ( 'NONE', *, *, #11068, .F. ) ;
#16315 =( BOUNDED_CURVE ( )  B_SPLINE_CURVE ( 2, ( #3093, #9016, #4474, #5863, #14312, #1611, #11696, #11885, #16082 ),
 .UNSPECIFIED., .F., .T. ) 
 B_SPLINE_CURVE_WITH_KNOTS ( ( 3, 2, 2, 2, 3 ),
 ( 0.3189655172413793371, 0.3218390804597701105, 0.3275862068965517127, 0.3333333333333333148, 0.3362068965517241437 ),
 .UNSPECIFIED. ) 
 CURVE ( )  GEOMETRIC_REPRESENTATION_ITEM ( )  RATIONAL_B_SPLINE_CURVE ( ( 0.9330127018922194093, 0.9330127018922200755, 1.000000000000000000, 0.8660254037844387076, 1.000000000000000000, 0.8660254037844387076, 1.000000000000000000, 0.9330127018922187432, 0.9330127018922194093 ) ) 
 REPRESENTATION_ITEM ( '' )  );
#16316 = DIRECTION ( 'NONE',  ( -0.000000000000000000, 1.000000000000000000, -0.000000000000000000 ) ) ;
#16317 = CARTESIAN_POINT ( 'NONE',  ( 4.518350579753602325, 30.62819992234354416, -1.405661355842793725 ) ) ;
#16318 = CARTESIAN_POINT ( 'NONE',  ( -3.518350579753606322, 34.37819992234354771, 1.080741659609877781 ) ) ;
#16319 = CARTESIAN_POINT ( 'NONE',  ( 0.8262555684460829442, 20.25319992234354771, -2.360188852285421302 ) ) ;
#16320 = ORIENTED_EDGE ( 'NONE', *, *, #2712, .F. ) ;
#16321 = CARTESIAN_POINT ( 'NONE',  ( -1.444289557196047014, 18.49680007765647360, -4.262301884875704161 ) ) ;
#16322 = EDGE_CURVE ( 'NONE', #9296, #218, #16103, .T. ) ;
#16323 = CARTESIAN_POINT ( 'NONE',  ( -2.000000000000005773, -25.22687694484738685, -5.706757097073694496 ) ) ;
#16324 = ORIENTED_EDGE ( 'NONE', *, *, #3332, .T. ) ;
#16325 = AXIS2_PLACEMENT_3D ( 'NONE', #12295, #644, #5255 ) ;
#16326 = CARTESIAN_POINT ( 'NONE',  ( 0.000000000000000000, 5.977523610840987267, 32.81826849749789687 ) ) ;
#16327 = CARTESIAN_POINT ( 'NONE',  ( -0.05938372350927861171, 38.62180007765648071, -3.680117784833935701 ) ) ;
#16328 = CARTESIAN_POINT ( 'NONE',  ( 10.00000000000000355, 25.39999999999999503, 2.499999999999996891 ) ) ;
#16329 = CARTESIAN_POINT ( 'NONE',  ( -5.330712181944246111E-15, -23.68761282235488252, -1.004956746021377967 ) ) ;
#16330 = CARTESIAN_POINT ( 'NONE',  ( -2.121784821875005722, -27.12577341693091171, -8.050904001845182734 ) ) ;
#16331 = CARTESIAN_POINT ( 'NONE',  ( -3.706921591972381904E-14, -19.73640722255826319, -10.87881775021074127 ) ) ;
#16332 = ORIENTED_EDGE ( 'NONE', *, *, #7503, .F. ) ;
#16333 = CARTESIAN_POINT ( 'NONE',  ( 6.428571428571431490, -11.73421655796352248, 14.25837509840157757 ) ) ;
#16334 = CARTESIAN_POINT ( 'NONE',  ( 8.500000000000001776, 15.00000000000000178, -20.49999999999999645 ) ) ;
#16335 = CARTESIAN_POINT ( 'NONE',  ( 4.243569643750000786, -26.86852450816387972, -14.09074965301504534 ) ) ;
#16336 = ORIENTED_EDGE ( 'NONE', *, *, #3559, .T. ) ;
#16337 = CARTESIAN_POINT ( 'NONE',  ( 3.481649420246394122, 23.37819992234353705, 1.193696214020467439 ) ) ;
#16338 = DIRECTION ( 'NONE',  ( 0.000000000000000000, -0.000000000000000000, -1.000000000000000000 ) ) ;
#16339 = CARTESIAN_POINT ( 'NONE',  ( -4.243569643750005227, -22.75612477167838676, -3.946144054785039490 ) ) ;
#16340 = CARTESIAN_POINT ( 'NONE',  ( -1.593127413382998459, 25.87180007765647716, -2.091722143975139669 ) ) ;
#16341 = CARTESIAN_POINT ( 'NONE',  ( -1.135272562821019626, 39.00319992234354061, 3.311245368580577164 ) ) ;
#16342 =( BOUNDED_CURVE ( )  B_SPLINE_CURVE ( 2, ( #2543, #13836, #17008, #18308, #9747, #7319, #2894, #7140, #194 ),
 .UNSPECIFIED., .F., .F. ) 
 B_SPLINE_CURVE_WITH_KNOTS ( ( 3, 2, 2, 2, 3 ),
 ( 0.3534482758620690057, 0.3563218390804597790, 0.3620689655172413812, 0.3678160919540229834, 0.3706896551724138122 ),
 .UNSPECIFIED. ) 
 CURVE ( )  GEOMETRIC_REPRESENTATION_ITEM ( )  RATIONAL_B_SPLINE_CURVE ( ( 0.9330127018922194093, 0.9330127018922200755, 1.000000000000000000, 0.8660254037844387076, 1.000000000000000000, 0.8660254037844387076, 1.000000000000000000, 0.9330127018922187432, 0.9330127018922194093 ) ) 
 REPRESENTATION_ITEM ( '' )  );
#16343 = CARTESIAN_POINT ( 'NONE',  ( 4.000000000000003553, -25.03592396470017434, -15.49984274679136576 ) ) ;
#16344 = ORIENTED_EDGE ( 'NONE', *, *, #13386, .F. ) ;
#16345 = CARTESIAN_POINT ( 'NONE',  ( -2.121784821874996396, -18.09366551958387248, -7.966187446493337987 ) ) ;
#16346 = CARTESIAN_POINT ( 'NONE',  ( -2.798362969681365886, 17.74680007765647716, 2.102939460078824929 ) ) ;
#16347 =( GEOMETRIC_REPRESENTATION_CONTEXT ( 3 ) GLOBAL_UNCERTAINTY_ASSIGNED_CONTEXT ( ( #16605 ) ) GLOBAL_UNIT_ASSIGNED_CONTEXT ( ( #2229, #3778, #2408 ) ) REPRESENTATION_CONTEXT ( 'NONE', 'WORKASPACE' ) );
#16348 = AXIS2_PLACEMENT_3D ( 'NONE', #3018, #13958, #9780 ) ;
#16349 = DIRECTION ( 'NONE',  ( -1.000000000000000000, 0.000000000000000000, 0.000000000000000000 ) ) ;
#16350 = EDGE_CURVE ( 'NONE', #8594, #12622, #8876, .T. ) ;
#16351 = CARTESIAN_POINT ( 'NONE',  ( -2.694913683823400241, -15.45745613286698372, -10.86990606519495373 ) ) ;
#16352 = ADVANCED_FACE ( 'NONE', ( #18233 ), #6802, .F. ) ;
#16353 = CARTESIAN_POINT ( 'NONE',  ( 14.20000000000000107, 0.000000000000000000, 1.610000000000000098 ) ) ;
#16354 = VERTEX_POINT ( 'NONE', #5502 ) ;
#16355 = VERTEX_POINT ( 'NONE', #1159 ) ;
#16356 =( NAMED_UNIT ( * ) PLANE_ANGLE_UNIT ( ) SI_UNIT ( $, .RADIAN. ) );
#16357 = AXIS2_PLACEMENT_3D ( 'NONE', #15405, #4068, #6938 ) ;
#16358 = CARTESIAN_POINT ( 'NONE',  ( 2.000000000000004441, -17.87391402919079653, -7.284591486665584981 ) ) ;
#16359 = DIRECTION ( 'NONE',  ( 0.000000000000000000, 0.000000000000000000, -1.000000000000000000 ) ) ;
#16360 = ADVANCED_FACE ( 'NONE', ( #6707 ), #5034, .T. ) ;
#16361 = ORIENTED_EDGE ( 'NONE', *, *, #13512, .T. ) ;
#16362 = CIRCLE ( 'NONE', #15765, 2.000000000000000000 ) ;
#16363 = CARTESIAN_POINT ( 'NONE',  ( -0.7188294034286550893, 27.50319992234354771, -2.395093729190349130 ) ) ;
#16364 =( NAMED_UNIT ( * ) SI_UNIT ( $, .STERADIAN. ) SOLID_ANGLE_UNIT ( ) );
#16365 = CARTESIAN_POINT ( 'NONE',  ( 2.121784821875004390, -23.26660800492483006, -15.35391494592470885 ) ) ;
#16366 = CARTESIAN_POINT ( 'NONE',  ( 3.481649420246369697, 26.62180007765648071, -1.193696214020541824 ) ) ;
#16367 = AXIS2_PLACEMENT_3D ( 'NONE', #4506, #6175, #3309 ) ;
#16368 = EDGE_CURVE ( 'NONE', #6179, #4921, #10040, .T. ) ;
#16369 = CARTESIAN_POINT ( 'NONE',  ( 0.000000000000000000, 5.977523610840987267, 32.81826849749789687 ) ) ;
#16370 = CARTESIAN_POINT ( 'NONE',  ( -1.734723475976807094E-15, 18.79999999999999361, -2.500000000000000000 ) ) ;
#16371 = CARTESIAN_POINT ( 'NONE',  ( -2.121784821874996396, -22.48152525766933962, -14.23270058530414950 ) ) ;
#16372 = TOROIDAL_SURFACE ( 'NONE', #16079, 9.000000000000001776, 0.9999999999999991118 ) ;
#16373 = VECTOR ( 'NONE', #11751, 1000.000000000000000 ) ;
#16374 = DIRECTION ( 'NONE',  ( 0.000000000000000000, 0.8191520442889952403, -0.5735764363510413855 ) ) ;
#16375 = CARTESIAN_POINT ( 'NONE',  ( 1.444289557196047680, 19.74680007765647716, 4.262301884875704161 ) ) ;
#16376 = CARTESIAN_POINT ( 'NONE',  ( -2.465190328815646976E-33, -26.97786251599082519, -14.24690051095425858 ) ) ;
#16377 = PLANE ( 'NONE',  #15345 ) ;
#16378 = CARTESIAN_POINT ( 'NONE',  ( -4.243569643750005227, -25.07910933890011407, -7.263709834155468670 ) ) ;
#16379 = ORIENTED_EDGE ( 'NONE', *, *, #9727, .F. ) ;
#16380 = CARTESIAN_POINT ( 'NONE',  ( -8.500000000000005329, 15.00000000000000178, -20.49999999999999645 ) ) ;
#16381 = CARTESIAN_POINT ( 'NONE',  ( 9.000000000000001776, 36.39999999999999147, -2.500000000000002665 ) ) ;
#16382 = CARTESIAN_POINT ( 'NONE',  ( -1.593127413382998459, 33.37180007765648071, -2.091722143975139669 ) ) ;
#16383 = EDGE_LOOP ( 'NONE', ( #1010, #3059, #10935, #13184 ) ) ;
#16384 = CARTESIAN_POINT ( 'NONE',  ( -0.05938372350927861865, 28.62180007765647716, -3.680117784833935701 ) ) ;
#16385 = CARTESIAN_POINT ( 'NONE',  ( 1.533898589781675205E-14, -28.48355344591296401, -9.423462828807814162 ) ) ;
#16386 = AXIS2_PLACEMENT_3D ( 'NONE', #5941, #12556, #12891 ) ;
#16387 = SHAPE_DEFINITION_REPRESENTATION ( #16120, #4006 ) ;
#16388 = DIRECTION ( 'NONE',  ( -3.469446951953613696E-16, -0.000000000000000000, -1.000000000000000000 ) ) ;
#16389 = ORIENTED_EDGE ( 'NONE', *, *, #16016, .F. ) ;
#16390 = CARTESIAN_POINT ( 'NONE',  ( 4.243569643750000786, -23.25499295915232167, -8.930091773994377036 ) ) ;
#16391 = CARTESIAN_POINT ( 'NONE',  ( 2.798362969681366330, 21.49680007765647716, -2.102939460078824929 ) ) ;
#16392 = VERTEX_POINT ( 'NONE', #12452 ) ;
#16393 = CARTESIAN_POINT ( 'NONE',  ( 4.000000000000000000, 1.759474945355381514, -3.047500000000001652 ) ) ;
#16394 = EDGE_CURVE ( 'NONE', #1782, #5033, #12730, .T. ) ;
#16395 = CARTESIAN_POINT ( 'NONE',  ( 9.000000000000005329, 25.39999999999999503, 2.499999999999997335 ) ) ;
#16396 = CARTESIAN_POINT ( 'NONE',  ( 0.4841626239896907880, -23.78953207011253923, -16.78102399689576174 ) ) ;
#16397 = VECTOR ( 'NONE', #2208, 1000.000000000000000 ) ;
#16398 = PLANE ( 'NONE',  #7675 ) ;
#16399 = VECTOR ( 'NONE', #128, 1000.000000000000000 ) ;
#16400 = CARTESIAN_POINT ( 'NONE',  ( 2.000000000000004441, -21.74555497456032427, -12.81386778561629924 ) ) ;
#16401 = CARTESIAN_POINT ( 'NONE',  ( -2.121784821874996396, -17.06122793415199723, -6.491713766773147931 ) ) ;
#16402 = ORIENTED_EDGE ( 'NONE', *, *, #8455, .F. ) ;
#16403 = CARTESIAN_POINT ( 'NONE',  ( 4.299564228933482956E-15, -19.80093457235270549, -10.97097235620001854 ) ) ;
#16404 = CARTESIAN_POINT ( 'NONE',  ( -5.279047395330986450E-15, -26.73198927754956600, -5.843121321406028912 ) ) ;
#16405 = CARTESIAN_POINT ( 'NONE',  ( -1.135272562821090014, 30.99680007765647716, -3.311245368580554072 ) ) ;
#16406 = EDGE_LOOP ( 'NONE', ( #10622, #7113, #9455, #16530 ) ) ;
#16407 =( GEOMETRIC_REPRESENTATION_CONTEXT ( 3 ) GLOBAL_UNCERTAINTY_ASSIGNED_CONTEXT ( ( #12482 ) ) GLOBAL_UNIT_ASSIGNED_CONTEXT ( ( #443, #7753, #9328 ) ) REPRESENTATION_CONTEXT ( 'NONE', 'WORKASPACE' ) );
#16408 = ORIENTED_EDGE ( 'NONE', *, *, #12155, .F. ) ;
#16409 = DIRECTION ( 'NONE',  ( 0.000000000000000000, 0.000000000000000000, -1.000000000000000000 ) ) ;
#16410 = CARTESIAN_POINT ( 'NONE',  ( 4.481649420246397675, 35.87819992234354771, 1.518615910253363177 ) ) ;
#16411 = CARTESIAN_POINT ( 'NONE',  ( 3.500000000000000444, 33.25319992234354771, 0.05647727720529520379 ) ) ;
#16412 = CARTESIAN_POINT ( 'NONE',  ( 2.481649420246391902, 25.87819992234355126, 0.8687765177875720335 ) ) ;
#16413 = AXIS2_PLACEMENT_3D ( 'NONE', #16369, #3653, #7905 ) ;
#16414 = ORIENTED_EDGE ( 'NONE', *, *, #8742, .T. ) ;
#16415 = CARTESIAN_POINT ( 'NONE',  ( 3.607379964056306676, 26.49680007765647716, -2.690724712371305838 ) ) ;
#16416 = CARTESIAN_POINT ( 'NONE',  ( -4.000000000000000888, -20.88361287976100300, -5.543410040383684567 ) ) ;
#16417 = ORIENTED_EDGE ( 'NONE', *, *, #7137, .T. ) ;
#16418 = CARTESIAN_POINT ( 'NONE',  ( -1.999999999999996225, -18.86333338189633579, -8.697628763064102486 ) ) ;
#16419 = VECTOR ( 'NONE', #11764, 999.9999999999998863 ) ;
#16420 = CARTESIAN_POINT ( 'NONE',  ( -3.518350579753630747, 38.12180007765648071, -1.080741659609802729 ) ) ;
#16421 = CARTESIAN_POINT ( 'NONE',  ( 4.000000000000000888, -23.85187093787765278, -9.782521869579230867 ) ) ;
#16422 = CARTESIAN_POINT ( 'NONE',  ( -4.243569643750000786, -19.73825243377498850, -3.907665802447479297 ) ) ;
#16423 =( BOUNDED_CURVE ( )  B_SPLINE_CURVE ( 3, ( #10011, #17088, #1879, #4458 ),
 .UNSPECIFIED., .F., .F. ) 
 B_SPLINE_CURVE_WITH_KNOTS ( ( 4, 4 ),
 ( -8.881784197001252323E-16, 1.570796326794896558 ),
 .UNSPECIFIED. ) 
 CURVE ( )  GEOMETRIC_REPRESENTATION_ITEM ( )  RATIONAL_B_SPLINE_CURVE ( ( 1.000000000000000000, 0.8047378541243648264, 0.8047378541243648264, 1.000000000000000000 ) ) 
 REPRESENTATION_ITEM ( '' )  );
#16424 = CARTESIAN_POINT ( 'NONE',  ( 4.243569643749996345, -26.83210232249799532, -9.767243269513704362 ) ) ;
#16425 = PRODUCT ( 'Brass Valve Body', 'Brass Valve Body', '', ( #9231 ) ) ;
#16426 = CARTESIAN_POINT ( 'NONE',  ( -2.195159659341646030, -29.79542698874031714, -12.39207419899238083 ) ) ;
#16427 = EDGE_CURVE ( 'NONE', #12786, #9963, #12132, .T. ) ;
#16428 = ORIENTED_EDGE ( 'NONE', *, *, #2419, .F. ) ;
#16429 = CARTESIAN_POINT ( 'NONE',  ( -4.253155871621290274, -10.96494312749350364, 19.45022984308078406 ) ) ;
#16430 = CARTESIAN_POINT ( 'NONE',  ( -10.00000000000000178, 25.39999999999999503, -2.500000000000001776 ) ) ;
#16431 = FILL_AREA_STYLE_COLOUR ( '', #12789 ) ;
#16432 = CARTESIAN_POINT ( 'NONE',  ( -5.330712181944245322E-15, -30.43072080220681386, -10.63511296669387818 ) ) ;
#16433 = ORIENTED_EDGE ( 'NONE', *, *, #4160, .T. ) ;
#16434 = CARTESIAN_POINT ( 'NONE',  ( -3.500000000000000444, 37.00319992234354061, -0.05647727720529563400 ) ) ;
#16435 = ADVANCED_FACE ( 'NONE', ( #3841 ), #3932, .T. ) ;
#16436 = DIRECTION ( 'NONE',  ( -0.3258630558627198526, 0.000000000000000000, -0.9454169814551725004 ) ) ;
#16437 = CARTESIAN_POINT ( 'NONE',  ( -5.330712181944245322E-15, -24.46194101142878807, -2.110812005811521619 ) ) ;
#16438 = CARTESIAN_POINT ( 'NONE',  ( 2.481649420246374138, 29.12180007765648426, -0.8687765177876252132 ) ) ;
#16439 = CARTESIAN_POINT ( 'NONE',  ( 3.607379964056363075, 16.00319992234354416, 2.690724712371229010 ) ) ;
#16440 = CARTESIAN_POINT ( 'NONE',  ( 4.713407268011036227E-15, -21.03627994800016054, -13.81407702374171365 ) ) ;
#16441 = EDGE_LOOP ( 'NONE', ( #481, #15874, #410, #17418, #10766 ) ) ;
#16442 = CARTESIAN_POINT ( 'NONE',  ( 4.243569643750003451, -18.64544601037477278, -6.618466598754856101 ) ) ;
#16443 = CARTESIAN_POINT ( 'NONE',  ( -2.829195390882805139, 38.37180007765647360, -3.793023760679206102 ) ) ;
#16444 = CARTESIAN_POINT ( 'NONE',  ( 10.00000000000000000, 36.39999999999999147, -2.500000000000003109 ) ) ;
#16445 = DIRECTION ( 'NONE',  ( -3.469446951953613696E-16, -0.000000000000000000, -1.000000000000000000 ) ) ;
#16446 = CARTESIAN_POINT ( 'NONE',  ( -9.000000000000001776, 43.00000000000000000, 2.499999999999998224 ) ) ;
#16447 = ORIENTED_EDGE ( 'NONE', *, *, #4725, .F. ) ;
#16448 = ORIENTED_EDGE ( 'NONE', *, *, #4562, .T. ) ;
#16449 = CYLINDRICAL_SURFACE ( 'NONE', #7041, 0.9999999999999991118 ) ;
#16450 = DIRECTION ( 'NONE',  ( -0.000000000000000000, 1.000000000000000000, -0.000000000000000000 ) ) ;
#16451 = CARTESIAN_POINT ( 'NONE',  ( -5.577813053751546416E-15, -29.25788163498686245, -10.52931808859795559 ) ) ;
#16452 = EDGE_LOOP ( 'NONE', ( #12797, #1770, #1217, #2630 ) ) ;
#16453 = CARTESIAN_POINT ( 'NONE',  ( 2.518350579753611207, 33.12819992234354771, -0.7558219633769606149 ) ) ;
#16454 = CARTESIAN_POINT ( 'NONE',  ( 4.243569643749996345, -25.76740106252136542, -8.246692287302257895 ) ) ;
#16455 = CARTESIAN_POINT ( 'NONE',  ( -1.027846397803541700, 19.99680007765648071, 3.346150245485522312 ) ) ;
#16456 = DIRECTION ( 'NONE',  ( 1.000000000000000000, 0.000000000000000000, 0.000000000000000000 ) ) ;
#16457 = FACE_OUTER_BOUND ( 'NONE', #712, .T. ) ;
#16458 = ADVANCED_FACE ( 'NONE', ( #9764 ), #9487, .T. ) ;
#16459 = CARTESIAN_POINT ( 'NONE',  ( 4.243569643749996345, -26.83210232249799532, -9.767243269513704362 ) ) ;
#16460 = EDGE_CURVE ( 'NONE', #2227, #6288, #16595, .T. ) ;
#16461 = FACE_BOUND ( 'NONE', #18009, .T. ) ;
#16462 = CARTESIAN_POINT ( 'NONE',  ( -2.829195390882805139, 25.87180007765647716, -3.793023760679206102 ) ) ;
#16463 = PLANE ( 'NONE',  #18019 ) ;
#16464 = CARTESIAN_POINT ( 'NONE',  ( -2.121784821875005722, -24.77052517516444752, -4.687260919983497587 ) ) ;
#16465 = CIRCLE ( 'NONE', #10533, 8.000000000000001776 ) ;
#16466 = ORIENTED_EDGE ( 'NONE', *, *, #6077, .T. ) ;
#16467 = LINE ( 'NONE', #12090, #15727 ) ;
#16468 = CARTESIAN_POINT ( 'NONE',  ( -8.000000000000001776, 38.59999999999999432, 2.499999999999998224 ) ) ;
#16469 = CARTESIAN_POINT ( 'NONE',  ( 8.000000000000000000, 43.00000000000000000, 2.500000000000000000 ) ) ;
#16470 = CARTESIAN_POINT ( 'NONE',  ( 0.05938372350926800214, 29.87180007765648426, 2.628655560595669183 ) ) ;
#16471 = CIRCLE ( 'NONE', #9345, 0.9999999999999991118 ) ;
#16472 = CARTESIAN_POINT ( 'NONE',  ( 1.071796769724504328, -23.82605761075068429, -2.771869435411045579 ) ) ;
#16473 = CARTESIAN_POINT ( 'NONE',  ( -2.115076519116362519, 30.12180007765647716, 3.012182706137108035 ) ) ;
#16474 = DIRECTION ( 'NONE',  ( 0.000000000000000000, 0.000000000000000000, -1.000000000000000000 ) ) ;
#16475 =( LENGTH_UNIT ( ) NAMED_UNIT ( * ) SI_UNIT ( .MILLI., .METRE. ) );
#16476 = DIRECTION ( 'NONE',  ( 0.000000000000000000, 0.000000000000000000, -1.000000000000000000 ) ) ;
#16477 = EDGE_CURVE ( 'NONE', #10311, #16492, #11148, .T. ) ;
#16478 = EDGE_CURVE ( 'NONE', #10466, #8695, #18323, .T. ) ;
#16479 = ORIENTED_EDGE ( 'NONE', *, *, #8967, .T. ) ;
#16480 = CARTESIAN_POINT ( 'NONE',  ( -4.243569643750004339, -23.56271663529704696, -5.098076617066439553 ) ) ;
#16481 = CARTESIAN_POINT ( 'NONE',  ( 2.864755990943265829, 26.99680007765648071, 2.011557305968487697 ) ) ;
#16482 = EDGE_CURVE ( 'NONE', #11926, #5429, #11527, .T. ) ;
#16483 = ORIENTED_EDGE ( 'NONE', *, *, #4559, .T. ) ;
#16484 = AXIS2_PLACEMENT_3D ( 'NONE', #9473, #3821, #9569 ) ;
#16485 = DIRECTION ( 'NONE',  ( 0.000000000000000000, 0.000000000000000000, -1.000000000000000000 ) ) ;
#16486 = AXIS2_PLACEMENT_3D ( 'NONE', #8386, #6820, #1183 ) ;
#16487 = FACE_OUTER_BOUND ( 'NONE', #12743, .T. ) ;
#16488 = CARTESIAN_POINT ( 'NONE',  ( 1.761081750400359969, -24.08916239126616787, -16.59049792717877736 ) ) ;
#16489 = CARTESIAN_POINT ( 'NONE',  ( 9.350658029750295697, -10.00000000000000178, 13.61865533257045691 ) ) ;
#16490 = CARTESIAN_POINT ( 'NONE',  ( 4.150834101209824212, -27.15734369766470380, -14.50322620280942587 ) ) ;
#16491 = CARTESIAN_POINT ( 'NONE',  ( 4.243569643750003451, -17.87111782130087434, -5.512611338964712893 ) ) ;
#16492 = VERTEX_POINT ( 'NONE', #16562 ) ;
#16493 = DIRECTION ( 'NONE',  ( 0.000000000000000000, 0.000000000000000000, -1.000000000000000000 ) ) ;
#16494 = CARTESIAN_POINT ( 'NONE',  ( -4.000000000000004441, -25.14136629352392660, -7.597794184370155079 ) ) ;
#16495 = CARTESIAN_POINT ( 'NONE',  ( 2.115076519116362963, 31.37180007765647716, -3.012182706137107147 ) ) ;
#16496 = ORIENTED_EDGE ( 'NONE', *, *, #10577, .T. ) ;
#16497 = EDGE_LOOP ( 'NONE', ( #13412, #7694 ) ) ;
#16498 = CARTESIAN_POINT ( 'NONE',  ( -1.734723475976807094E-15, 18.79999999999999361, -2.500000000000000000 ) ) ;
#16499 = SHAPE_REPRESENTATION_RELATIONSHIP ( 'NONE' , 'NONE' ,  #7684, #18244 ) ;
#16500 = CARTESIAN_POINT ( 'NONE',  ( 3.607379964056363075, 31.00319992234354771, 2.690724712371229010 ) ) ;
#16501 = CARTESIAN_POINT ( 'NONE',  ( 2.000000000000004441, -20.71311738912845257, -11.33939410589610652 ) ) ;
#16502 = AXIS2_PLACEMENT_3D ( 'NONE', #15070, #8004, #14900 ) ;
#16503 = CARTESIAN_POINT ( 'NONE',  ( 0.7188294034286553114, 31.25319992234354416, 2.395093729190349130 ) ) ;
#16504 = ORIENTED_EDGE ( 'NONE', *, *, #6702, .F. ) ;
#16505 = CARTESIAN_POINT ( 'NONE',  ( -4.499999999999999112, 25.49680007765647716, 0.05647727720537927543 ) ) ;
#16506 = CARTESIAN_POINT ( 'NONE',  ( 4.000000000000000888, -21.01266757793999318, -5.727719250348704882 ) ) ;
#16507 = VERTEX_POINT ( 'NONE', #15163 ) ;
#16508 = DIRECTION ( 'NONE',  ( -4.915049848600951133E-16, 0.000000000000000000, -1.000000000000000000 ) ) ;
#16509 = CARTESIAN_POINT ( 'NONE',  ( 3.481649420246369697, 39.12180007765646650, -1.193696214020541824 ) ) ;
#16510 = DIRECTION ( 'NONE',  ( -0.000000000000000000, -0.000000000000000000, -1.000000000000000000 ) ) ;
#16511 = EDGE_CURVE ( 'NONE', #9790, #7280, #1341, .T. ) ;
#16512 = CARTESIAN_POINT ( 'NONE',  ( 2.121784821875004390, -16.81387309597561242, -6.138454447673516334 ) ) ;
#16513 = VECTOR ( 'NONE', #8472, 1000.000000000000000 ) ;
#16514 = CARTESIAN_POINT ( 'NONE',  ( -5.330712181944245322E-15, -28.62395502770104017, -8.054784027183542250 ) ) ;
#16515 = DIRECTION ( 'NONE',  ( 1.000000000000000000, 0.000000000000000000, 0.000000000000000000 ) ) ;
#16516 = ORIENTED_EDGE ( 'NONE', *, *, #12270, .F. ) ;
#16517 = LINE ( 'NONE', #4167, #8935 ) ;
#16518 = CARTESIAN_POINT ( 'NONE',  ( -8.500000000000010658, 13.00000000000000178, 22.64999999999998437 ) ) ;
#16519 = DIRECTION ( 'NONE',  ( -1.000000000000000000, 0.000000000000000000, 0.000000000000000000 ) ) ;
#16520 = CARTESIAN_POINT ( 'NONE',  ( 4.243569643750000786, -26.35230571544794387, -13.35351281315494987 ) ) ;
#16521 = ORIENTED_EDGE ( 'NONE', *, *, #7835, .T. ) ;
#16522 = CARTESIAN_POINT ( 'NONE',  ( 2.798362969681409851, 38.50319992234354061, 2.102939460078764977 ) ) ;
#16523 = CARTESIAN_POINT ( 'NONE',  ( 0.000000000000000000, 10.00000000000000000, 0.000000000000000000 ) ) ;
#16524 = CARTESIAN_POINT ( 'NONE',  ( 4.730628863548789710E-15, -15.78889204519509981, -6.810374858873577075 ) ) ;
#16525 = CARTESIAN_POINT ( 'NONE',  ( -2.481649420246374138, 32.87180007765648071, 0.8687765177876256573 ) ) ;
#16526 = AXIS2_PLACEMENT_3D ( 'NONE', #14126, #5601, #11418 ) ;
#16527 = CARTESIAN_POINT ( 'NONE',  ( 4.518350579753602325, 28.12819992234354416, -1.405661355842793725 ) ) ;
#16528 = AXIS2_PLACEMENT_3D ( 'NONE', #16583, #13688, #16307 ) ;
#16529 = CARTESIAN_POINT ( 'NONE',  ( -4.000000000000000888, -25.01336322148850044, -11.44130475926444745 ) ) ;
#16530 = ORIENTED_EDGE ( 'NONE', *, *, #16482, .T. ) ;
#16531 = EDGE_CURVE ( 'NONE', #7975, #2685, #14822, .T. ) ;
#16532 = CARTESIAN_POINT ( 'NONE',  ( -3.999999999999997335, -23.72386786725210328, -13.62603244648705925 ) ) ;
#16533 = CARTESIAN_POINT ( 'NONE',  ( -4.481649420246366589, 40.37180007765647360, 1.518615910253458878 ) ) ;
#16534 =( BOUNDED_CURVE ( )  B_SPLINE_CURVE ( 2, ( #7310, #6020, #17825, #13251, #16421, #5087, #3614, #570, #16148 ),
 .UNSPECIFIED., .F., .T. ) 
 B_SPLINE_CURVE_WITH_KNOTS ( ( 3, 2, 2, 2, 3 ),
 ( 0.4396551724137931494, 0.4425287356321839227, 0.4482758620689655249, 0.4540229885057471271, 0.4568965517241379559 ),
 .UNSPECIFIED. ) 
 CURVE ( )  GEOMETRIC_REPRESENTATION_ITEM ( )  RATIONAL_B_SPLINE_CURVE ( ( 0.9330127018922194093, 0.9330127018922200755, 1.000000000000000000, 0.8660254037844387076, 1.000000000000000000, 0.8660254037844387076, 1.000000000000000000, 0.9330127018922187432, 0.9330127018922194093 ) ) 
 REPRESENTATION_ITEM ( '' )  );
#16535 = EDGE_CURVE ( 'NONE', #3185, #11364, #2738, .T. ) ;
#16536 = CARTESIAN_POINT ( 'NONE',  ( 4.730628863548789710E-15, -20.43486117963853133, -13.44550641761443543 ) ) ;
#16537 = AXIS2_PLACEMENT_3D ( 'NONE', #12739, #3193, #11422 ) ;
#16538 = CLOSED_SHELL ( 'NONE', ( #1675, #5477, #13952, #1473, #3992, #1157, #9435, #1050, #6084, #12544 ) ) ;
#16539 = CARTESIAN_POINT ( 'NONE',  ( -6.158835246850665095E-15, -22.83371997885389604, -15.30223878937131587 ) ) ;
#16540 = FACE_OUTER_BOUND ( 'NONE', #5899, .T. ) ;
#16541 = CYLINDRICAL_SURFACE ( 'NONE', #853, 4.000000000000000000 ) ;
#16542 = EDGE_LOOP ( 'NONE', ( #1291, #393 ) ) ;
#16543 = AXIS2_PLACEMENT_3D ( 'NONE', #617, #6256, #11909 ) ;
#16544 = VERTEX_POINT ( 'NONE', #9582 ) ;
#16545 = CARTESIAN_POINT ( 'NONE',  ( -2.798362969681365886, 17.74680007765647716, 2.102939460078824929 ) ) ;
#16546 = DIRECTION ( 'NONE',  ( 0.000000000000000000, 0.000000000000000000, 1.000000000000000000 ) ) ;
#16547 = CARTESIAN_POINT ( 'NONE',  ( 8.500000000000001776, 14.80000000000000071, -20.49999999999999645 ) ) ;
#16548 = CARTESIAN_POINT ( 'NONE',  ( 1.071796769724485454, -20.78037150870897065, -12.36975326458684954 ) ) ;
#16549 = ORIENTED_EDGE ( 'NONE', *, *, #8011, .T. ) ;
#16550 = CARTESIAN_POINT ( 'NONE',  ( 2.500000000000001332, 38.25319992234354771, 0.05647727720530566764 ) ) ;
#16551 = CARTESIAN_POINT ( 'NONE',  ( -4.243569643750000786, -24.90044036093436119, -11.28003420104843357 ) ) ;
#16552 = CARTESIAN_POINT ( 'NONE',  ( 0.05938372350927906274, 29.87180007765648071, 3.680117784833935701 ) ) ;
#16553 = CARTESIAN_POINT ( 'NONE',  ( 2.864755990943222308, 28.00319992234354416, -2.011557305968548093 ) ) ;
#16554 = FACE_OUTER_BOUND ( 'NONE', #169, .T. ) ;
#16555 = DIRECTION ( 'NONE',  ( 3.469446951953612217E-16, -0.000000000000000000, 1.000000000000000000 ) ) ;
#16556 = AXIS2_PLACEMENT_3D ( 'NONE', #17282, #15971, #3264 ) ;
#16557 = CARTESIAN_POINT ( 'NONE',  ( -5.330712181944245322E-15, -27.84962683862713106, -6.948928767393398154 ) ) ;
#16558 = EDGE_CURVE ( 'NONE', #1458, #3584, #13698, .T. ) ;
#16559 = AXIS2_PLACEMENT_3D ( 'NONE', #10305, #15988, #14597 ) ;
#16560 = CARTESIAN_POINT ( 'NONE',  ( 4.898587196589413815E-16, 2.700915433685006750, 35.11257424290206330 ) ) ;
#16561 = CARTESIAN_POINT ( 'NONE',  ( -4.481649420246366589, 25.37180007765648426, 1.518615910253458878 ) ) ;
#16562 = CARTESIAN_POINT ( 'NONE',  ( 13.00000000000000178, 13.00000000000000178, 25.00000000000000355 ) ) ;
#16563 = CARTESIAN_POINT ( 'NONE',  ( -8.500000000000005329, 15.00000000000000178, -22.64999999999999147 ) ) ;
#16564 = CARTESIAN_POINT ( 'NONE',  ( -2.121784821874996396, -18.31951124139709464, -8.288728563932130200 ) ) ;
#16565 = ORIENTED_EDGE ( 'NONE', *, *, #207, .F. ) ;
#16566 = CARTESIAN_POINT ( 'NONE',  ( 1.999999999999994449, -28.08758942185315988, -9.792277918971819872 ) ) ;
#16567 = CIRCLE ( 'NONE', #1454, 2.149999999999999023 ) ;
#16568 = CARTESIAN_POINT ( 'NONE',  ( 1.989345975306426206, 38.99680007765648071, -1.515154207786343799 ) ) ;
#16569 = CARTESIAN_POINT ( 'NONE',  ( 4.000000000000003553, -18.58318905575096025, -6.284382248540171467 ) ) ;
#16570 = CARTESIAN_POINT ( 'NONE',  ( 3.481649420246370141, 39.12180007765646650, -1.193696214020541602 ) ) ;
#16571 = CARTESIAN_POINT ( 'NONE',  ( 20.00000000000000355, 0.000000000000000000, 0.000000000000000000 ) ) ;
#16572 = APPLICATION_PROTOCOL_DEFINITION ( 'draft international standard', 'automotive_design', 1998, #7947 ) ;
#16573 = CARTESIAN_POINT ( 'NONE',  ( -3.706921591972381904E-14, -18.18775084441045209, -8.667107230630458403 ) ) ;
#16574 = VERTEX_POINT ( 'NONE', #310 ) ;
#16576 = CARTESIAN_POINT ( 'NONE',  ( -2.121784821874996396, -17.83555612322590278, -7.597569026563290251 ) ) ;
#16575 = AXIS2_PLACEMENT_3D ( 'NONE', #1450, #7081, #12747 ) ;
#16577 = CARTESIAN_POINT ( 'NONE',  ( -1.027846397803541700, 24.99680007765647716, 3.346150245485522312 ) ) ;
#16578 = ORIENTED_EDGE ( 'NONE', *, *, #12834, .T. ) ;
#16579 = CIRCLE ( 'NONE', #9754, 6.000000000000000000 ) ;
#16580 = DIRECTION ( 'NONE',  ( 1.000000000000000000, 0.000000000000000000, 0.000000000000000000 ) ) ;
#16581 = CARTESIAN_POINT ( 'NONE',  ( -2.121784821874996396, -23.73980856491443703, -16.02971538246313443 ) ) ;
#16582 = CARTESIAN_POINT ( 'NONE',  ( -1.071796769724486786, -19.20866172912349867, -10.12511907569473379 ) ) ;
#16583 = CARTESIAN_POINT ( 'NONE',  ( -1.734723475976807094E-15, 34.19999999999999574, -2.500000000000000000 ) ) ;
#16584 = CARTESIAN_POINT ( 'NONE',  ( 4.243569643750000786, -25.80382324818726048, -12.57019867080359710 ) ) ;
#16585 = EDGE_CURVE ( 'NONE', #13964, #4808, #1195, .T. ) ;
#16586 = VERTEX_POINT ( 'NONE', #120 ) ;
#16587 = CARTESIAN_POINT ( 'NONE',  ( 8.000000000000005329, 40.79999999999999716, 2.499999999999997780 ) ) ;
#16588 = CARTESIAN_POINT ( 'NONE',  ( -1.999999999999996225, -18.66975133533280484, -8.421164949123328469 ) ) ;
#16589 = VECTOR ( 'NONE', #1904, 1000.000000000000000 ) ;
#16590 = CARTESIAN_POINT ( 'NONE',  ( -2.055738996568313048, 18.24680007765647716, -1.423772053676023441 ) ) ;
#16591 = EDGE_CURVE ( 'NONE', #5029, #2896, #17201, .T. ) ;
#16592 = ORIENTED_EDGE ( 'NONE', *, *, #16350, .T. ) ;
#16593 = ORIENTED_EDGE ( 'NONE', *, *, #17049, .T. ) ;
#16594 = EDGE_CURVE ( 'NONE', #9655, #15102, #1800, .T. ) ;
#16595 = CIRCLE ( 'NONE', #2957, 4.000000000000000000 ) ;
#16596 = CARTESIAN_POINT ( 'NONE',  ( 0.05938372350919016857, 37.62819992234354771, -4.731580009072201776 ) ) ;
#16597 = UNCERTAINTY_MEASURE_WITH_UNIT (LENGTH_MEASURE( 1.000000000000000082E-05 ), #15648, 'distance_accuracy_value', 'NONE');
#16598 = CARTESIAN_POINT ( 'NONE',  ( 4.000000000000000000, -3.518949890710769246, 4.119968255444916849E-15 ) ) ;
#16599 = AXIS2_PLACEMENT_3D ( 'NONE', #18185, #5455, #12129 ) ;
#16600 = CARTESIAN_POINT ( 'NONE',  ( -0.05938372350921170689, 28.87819992234354416, 2.628655560595669183 ) ) ;
#16601 = ORIENTED_EDGE ( 'NONE', *, *, #7094, .F. ) ;
#16602 = CARTESIAN_POINT ( 'NONE',  ( -4.243569643750000786, -25.96514162091098399, -12.80058518325988182 ) ) ;
#16603 = EDGE_CURVE ( 'NONE', #13013, #5876, #4445, .T. ) ;
#16604 = CARTESIAN_POINT ( 'NONE',  ( 2.829195390882805583, 22.12180007765647716, 3.793023760679204770 ) ) ;
#16605 = UNCERTAINTY_MEASURE_WITH_UNIT (LENGTH_MEASURE( 1.000000000000000082E-05 ), #2229, 'distance_accuracy_value', 'NONE');
#16606 = CARTESIAN_POINT ( 'NONE',  ( -4.000000000000000888, -20.62550348340303685, -5.174791620453635943 ) ) ;
#16607 = ORIENTED_EDGE ( 'NONE', *, *, #16895, .F. ) ;
#16608 = CARTESIAN_POINT ( 'NONE',  ( 8.500000000000001776, 13.00000000000000000, -20.49999999999999645 ) ) ;
#16609 = CARTESIAN_POINT ( 'NONE',  ( -3.999999999999997335, -22.17521148910429574, -11.41432192690677283 ) ) ;
#16610 = ADVANCED_FACE ( 'NONE', ( #10115 ), #11695, .F. ) ;
#16611 = CARTESIAN_POINT ( 'NONE',  ( 8.500000000000019540, 10.00000000000000000, -20.49999999999998934 ) ) ;
#16612 = AXIS2_PLACEMENT_3D ( 'NONE', #2910, #14218, #17764 ) ;
#16613 = CARTESIAN_POINT ( 'NONE',  ( 4.243569643750003451, -18.09696354311409294, -5.835152456403505106 ) ) ;
#16614 = CARTESIAN_POINT ( 'NONE',  ( 4.730628863548789710E-15, -18.14414028696156933, -10.17401794073526311 ) ) ;
#16615 = PRODUCT_RELATED_PRODUCT_CATEGORY ( 'part', '', ( #13293 ) ) ;
#16616 = DIRECTION ( 'NONE',  ( -3.469446951953613696E-16, -0.000000000000000000, -1.000000000000000000 ) ) ;
#16617 = VERTEX_POINT ( 'NONE', #11508 ) ;
#16618 = CARTESIAN_POINT ( 'NONE',  ( 3.999999999999996447, -25.82965801714518506, -8.580776637516944305 ) ) ;
#16619 = CARTESIAN_POINT ( 'NONE',  ( -10.00000000000000178, 27.59999999999999432, -2.500000000000001776 ) ) ;
#16620 = LINE ( 'NONE', #15035, #9262 ) ;
#16621 = SURFACE_STYLE_FILL_AREA ( #2340 ) ;
#16622 = ORIENTED_EDGE ( 'NONE', *, *, #10080, .F. ) ;
#16623 = CARTESIAN_POINT ( 'NONE',  ( -1.135272562821019626, 36.50319992234354061, 3.311245368580577164 ) ) ;
#16624 = CARTESIAN_POINT ( 'NONE',  ( 2.798362969681409851, 23.50319992234354416, 2.102939460078764977 ) ) ;
#16625 = CARTESIAN_POINT ( 'NONE',  ( -4.000000000000004441, -28.75489784253548819, -12.75845206339082161 ) ) ;
#16626 = CARTESIAN_POINT ( 'NONE',  ( -0.7188294034286043521, 29.99680007765648071, 2.395093729190366005 ) ) ;
#16627 = AXIS2_PLACEMENT_3D ( 'NONE', #9691, #14146, #15634 ) ;
#16628 = CARTESIAN_POINT ( 'NONE',  ( -1.444289557195956863, 24.00319992234354416, 4.262301884875733471 ) ) ;
#16629 = UNCERTAINTY_MEASURE_WITH_UNIT (LENGTH_MEASURE( 1.000000000000000082E-05 ), #17586, 'distance_accuracy_value', 'NONE');
#16630 = CARTESIAN_POINT ( 'NONE',  ( 4.000000000000000888, -25.14241791966749417, -11.62561396922946777 ) ) ;
#16631 = ORIENTED_EDGE ( 'NONE', *, *, #6702, .T. ) ;
#16632 = CARTESIAN_POINT ( 'NONE',  ( -1.071796769724496334, -28.81771689278419757, -9.900697689383058275 ) ) ;
#16633 = CARTESIAN_POINT ( 'NONE',  ( 4.481649420246366589, 36.62180007765647360, -1.518615910253458212 ) ) ;
#16634 = CARTESIAN_POINT ( 'NONE',  ( 0.000000000000000000, 0.000000000000000000, 0.000000000000000000 ) ) ;
#16635 = CARTESIAN_POINT ( 'NONE',  ( -5.330712181944246111E-15, -28.59169135315629617, -8.008706724692286727 ) ) ;
#16636 = CYLINDRICAL_SURFACE ( 'NONE', #10580, 2.499999999999999556 ) ;
#16637 = CIRCLE ( 'NONE', #16325, 0.9999999999999991118 ) ;
#16638 = CARTESIAN_POINT ( 'NONE',  ( -3.706921591972381904E-14, -19.54282517599473579, -10.60235393626997080 ) ) ;
#16639 = CARTESIAN_POINT ( 'NONE',  ( -1.071796769724477238, -26.49473232556249158, -6.583131910012619770 ) ) ;
#16640 = ORIENTED_EDGE ( 'NONE', *, *, #14069, .F. ) ;
#16641 = ORIENTED_EDGE ( 'NONE', *, *, #4289, .T. ) ;
#16642 = CARTESIAN_POINT ( 'NONE',  ( -0.05938372350927861171, 16.12180007765647716, -3.680117784833935701 ) ) ;
#16643 = CARTESIAN_POINT ( 'NONE',  ( -997.9783121635130101, 0.000000000000000000, 0.000000000000000000 ) ) ;
#16644 = CARTESIAN_POINT ( 'NONE',  ( 1.071796769724494114, -23.42599282208309930, -16.14809206987660062 ) ) ;
#16645 = CARTESIAN_POINT ( 'NONE',  ( 7.401749373187970882, -13.34905268700159020, 2.825469154945078554 ) ) ;
#16646 = ORIENTED_EDGE ( 'NONE', *, *, #14092, .F. ) ;
#16647 = CARTESIAN_POINT ( 'NONE',  ( 2.055738996568281518, 33.00319992234354771, -1.423772053676066518 ) ) ;
#16648 = CARTESIAN_POINT ( 'NONE',  ( 2.121784821875004390, -20.94362343770310986, -12.03634916655427922 ) ) ;
#16649 = CARTESIAN_POINT ( 'NONE',  ( -1.135272562821090014, 33.49680007765648071, -3.311245368580554072 ) ) ;
#16650 = CARTESIAN_POINT ( 'NONE',  ( 1.027846397803612311, 23.75319992234354416, 3.346150245485499219 ) ) ;
#16651 = FACE_OUTER_BOUND ( 'NONE', #4456, .T. ) ;
#16652 = DIRECTION ( 'NONE',  ( 0.000000000000000000, -0.5735764363510413855, -0.8191520442889951292 ) ) ;
#16653 = CARTESIAN_POINT ( 'NONE',  ( 4.243569643750000786, -23.77121175186825752, -9.667328613854474284 ) ) ;
#16654 = FACE_OUTER_BOUND ( 'NONE', #13027, .T. ) ;
#16655 = CARTESIAN_POINT ( 'NONE',  ( -2.829195390882805139, 20.87180007765647716, -3.793023760679206102 ) ) ;
#16656 = CARTESIAN_POINT ( 'NONE',  ( -11.99999999999999822, 48.00000000000000000, -15.00000000000000000 ) ) ;
#16657 = DIRECTION ( 'NONE',  ( 0.000000000000000000, 0.000000000000000000, 1.000000000000000000 ) ) ;
#16658 = CARTESIAN_POINT ( 'NONE',  ( 4.243569643750003451, -19.90372931761987019, -8.415481395913838369 ) ) ;
#16659 = CARTESIAN_POINT ( 'NONE',  ( 0.000000000000000000, 5.977523610840987267, 32.81826849749789687 ) ) ;
#16660 = DIRECTION ( 'NONE',  ( 0.000000000000000000, 0.000000000000000000, -1.000000000000000000 ) ) ;
#16661 = CARTESIAN_POINT ( 'NONE',  ( 0.7188294034286049072, 38.74680007765646650, -2.395093729190366005 ) ) ;
#16662 = EDGE_CURVE ( 'NONE', #9284, #177, #17520, .T. ) ;
#16663 = CYLINDRICAL_SURFACE ( 'NONE', #15049, 0.9999999999999991118 ) ;
#16664 = CARTESIAN_POINT ( 'NONE',  ( -3.500000000000000444, 37.99680007765647360, 0.05647727720536892260 ) ) ;
#16665 = PLANE ( 'NONE',  #3046 ) ;
#16666 = CARTESIAN_POINT ( 'NONE',  ( -3.982427978483248587, 15.00000000000000355, -0.4169694339699933638 ) ) ;
#16667 = VERTEX_POINT ( 'NONE', #15798 ) ;
#16668 = CARTESIAN_POINT ( 'NONE',  ( -4.243569643749998122, -19.84995652671195643, -8.338685891761750568 ) ) ;
#16669 = CARTESIAN_POINT ( 'NONE',  ( -3.500000000000000444, 27.99680007765648071, 0.05647727720536892260 ) ) ;
#16670 = CIRCLE ( 'NONE', #11595, 8.000000000000000000 ) ;
#16671 = FACE_OUTER_BOUND ( 'NONE', #3343, .T. ) ;
#16672 = FACE_OUTER_BOUND ( 'NONE', #9233, .T. ) ;
#16673 = CARTESIAN_POINT ( 'NONE',  ( -4.016207988404787876, -26.68874843910498740, -14.64799399452802398 ) ) ;
#16674 = CARTESIAN_POINT ( 'NONE',  ( 4.299564228933482956E-15, -23.09182937521185863, -15.67085720930136006 ) ) ;
#16675 = CARTESIAN_POINT ( 'NONE',  ( -3.999999999999997335, -19.85222692188257554, -8.096756147536344983 ) ) ;
#16676 = CARTESIAN_POINT ( 'NONE',  ( 2.121784821874994176, -29.37347607688156259, -11.26095607540267807 ) ) ;
#16677 = ORIENTED_EDGE ( 'NONE', *, *, #10691, .T. ) ;
#16678 = CARTESIAN_POINT ( 'NONE',  ( 1.300000000000000044, 0.000000000000000000, -1.250000000000000000 ) ) ;
#16679 = CIRCLE ( 'NONE', #15498, 8.000000000000001776 ) ;
#16680 = CARTESIAN_POINT ( 'NONE',  ( 3.999999999999996447, -22.99045465720752901, -4.525974018286417433 ) ) ;
#16681 = AXIS2_PLACEMENT_3D ( 'NONE', #11655, #17349, #10259 ) ;
#16682 = CARTESIAN_POINT ( 'NONE',  ( 2.798362969681366330, 38.99680007765647360, -2.102939460078824929 ) ) ;
#16683 = ORIENTED_EDGE ( 'NONE', *, *, #1230, .F. ) ;
#16684 = CARTESIAN_POINT ( 'NONE',  ( -3.999999999999997335, -19.27148077937220449, -7.267364701686970463 ) ) ;
#16685 = CARTESIAN_POINT ( 'NONE',  ( -2.829195390882724315, 31.62819992234354416, 3.793023760679264722 ) ) ;
#16686 = CARTESIAN_POINT ( 'NONE',  ( 8.499999999999994671, 15.00000000000000178, 22.64999999999999147 ) ) ;
#16687 = CARTESIAN_POINT ( 'NONE',  ( -2.055738996568281518, 31.75319992234354771, 1.423772053676066962 ) ) ;
#16688 = ORIENTED_EDGE ( 'NONE', *, *, #15392, .T. ) ;
#16689 = CARTESIAN_POINT ( 'NONE',  ( -5.330712181944246111E-15, -29.39828321677494216, -9.160639286973685458 ) ) ;
#16690 = CARTESIAN_POINT ( 'NONE',  ( 1.444289557196047680, 27.24680007765647716, 4.262301884875704161 ) ) ;
#16691 = CARTESIAN_POINT ( 'NONE',  ( -2.000000000000005773, -23.16200177398363991, -2.757809737633313940 ) ) ;
#16692 = ORIENTED_EDGE ( 'NONE', *, *, #6615, .T. ) ;
#16693 = ADVANCED_FACE ( 'NONE', ( #4291 ), #3091, .F. ) ;
#16694 = CIRCLE ( 'NONE', #2763, 3.309499999999999886 ) ;
#16695 = EDGE_CURVE ( 'NONE', #3919, #12413, #13934, .T. ) ;
#16696 = CARTESIAN_POINT ( 'NONE',  ( 8.500000000000001776, 13.00000000000000178, -22.64999999999999147 ) ) ;
#16697 = MECHANICAL_DESIGN_GEOMETRIC_PRESENTATION_REPRESENTATION (  '', ( #2765 ), #8659 ) ;
#16698 = ADVANCED_BREP_SHAPE_REPRESENTATION ( '', ( #2427, #16940 ), #16347 ) ;
#16699 = SURFACE_STYLE_USAGE ( .BOTH. , #9710 ) ;
#16700 = CARTESIAN_POINT ( 'NONE',  ( 8.499999999999994671, 13.00000000000000178, 20.49999999999999645 ) ) ;
#16701 = CARTESIAN_POINT ( 'NONE',  ( -9.000000000000003553, 27.59999999999999432, -2.500000000000001776 ) ) ;
#16702 = CARTESIAN_POINT ( 'NONE',  ( -4.243569643750005227, -25.11137301344485451, -7.309787136646725081 ) ) ;
#16703 = ORIENTED_EDGE ( 'NONE', *, *, #1845, .F. ) ;
#16704 = CARTESIAN_POINT ( 'NONE',  ( 10.00000000000000355, 29.79999999999999716, 2.499999999999996891 ) ) ;
#16705 = ORIENTED_EDGE ( 'NONE', *, *, #16368, .T. ) ;
#16706 = CARTESIAN_POINT ( 'NONE',  ( 4.713407268011036227E-15, -20.06836971236272760, -12.43175795001079642 ) ) ;
#16707 = CARTESIAN_POINT ( 'NONE',  ( -3.481649420246370141, 17.87180007765647716, 1.193696214020542268 ) ) ;
#16708 = PRODUCT_DEFINITION_SHAPE ( 'NONE', 'NONE',  #18377 ) ;
#16709 = VECTOR ( 'NONE', #8202, 1000.000000000000000 ) ;
#16710 = FILL_AREA_STYLE ('',( #16431 ) ) ;
#16711 = ORIENTED_EDGE ( 'NONE', *, *, #6880, .F. ) ;
#16712 = CARTESIAN_POINT ( 'NONE',  ( -2.211161402132839182, 34.12819992234355482, 2.942372952327218627 ) ) ;
#16713 = CARTESIAN_POINT ( 'NONE',  ( -3.481649420246394566, 19.62819992234354416, -1.193696214020467883 ) ) ;
#16714 = CARTESIAN_POINT ( 'NONE',  ( -4.243569643750005227, -22.23990597896245447, -3.208907214924944462 ) ) ;
#16715 = CARTESIAN_POINT ( 'NONE',  ( -1.497042530366477164, 32.62180007765647360, 2.161531897785062384 ) ) ;
#16716 = ADVANCED_FACE ( 'NONE', ( #407 ), #10024, .F. ) ;
#16717 = CARTESIAN_POINT ( 'NONE',  ( -2.733110507866328476, 27.37819992234355126, -3.862833514489096398 ) ) ;
#16718 = CARTESIAN_POINT ( 'NONE',  ( -4.000000000000000888, -25.52958201420443984, -12.17854159912454293 ) ) ;
#16719 = VERTEX_POINT ( 'NONE', #2824 ) ;
#16720 = EDGE_CURVE ( 'NONE', #13359, #1006, #1799, .T. ) ;
#16721 = CARTESIAN_POINT ( 'NONE',  ( 4.243569643750000786, -20.15768020285669593, -4.506670734833804204 ) ) ;
#16722 = EDGE_CURVE ( 'NONE', #15166, #17010, #13333, .T. ) ;
#16723 = CARTESIAN_POINT ( 'NONE',  ( 1.135272562821090458, 24.74680007765647716, 3.311245368580554072 ) ) ;
#16724 = CIRCLE ( 'NONE', #3669, 0.9999999999999991118 ) ;
#16725 = CARTESIAN_POINT ( 'NONE',  ( -2.121784821875005722, -25.28674396788038337, -5.424497759843593059 ) ) ;
#16726 = CARTESIAN_POINT ( 'NONE',  ( -3.999999999999997335, -24.17555931017360393, -14.27111468035787922 ) ) ;
#16727 = FACE_OUTER_BOUND ( 'NONE', #11283, .T. ) ;
#16728 = DIRECTION ( 'NONE',  ( -4.915049848600951133E-16, 0.000000000000000000, -1.000000000000000000 ) ) ;
#16729 = EDGE_LOOP ( 'NONE', ( #17943, #17719, #9501, #13716, #10731 ) ) ;
#16730 = ORIENTED_EDGE ( 'NONE', *, *, #18156, .F. ) ;
#16731 = DIRECTION ( 'NONE',  ( -1.000000000000000000, 0.000000000000000000, 4.336808689942021680E-16 ) ) ;
#16732 = FACE_OUTER_BOUND ( 'NONE', #923, .T. ) ;
#16733 = DIRECTION ( 'NONE',  ( -0.000000000000000000, -1.000000000000000000, -0.000000000000000000 ) ) ;
#16734 = FACE_OUTER_BOUND ( 'NONE', #17302, .T. ) ;
#16735 = EDGE_LOOP ( 'NONE', ( #10121, #5963, #2959, #14412 ) ) ;
#16736 = CARTESIAN_POINT ( 'NONE',  ( 0.8262555684460829442, 32.75319992234354061, -2.360188852285421302 ) ) ;
#16737 = CARTESIAN_POINT ( 'NONE',  ( -4.243569643750005227, -26.88587511340589131, -9.844038773665802822 ) ) ;
#16738 = CARTESIAN_POINT ( 'NONE',  ( 3.518350579753631191, 29.37180007765647005, 1.080741659609802285 ) ) ;
#16739 = PRODUCT_DEFINITION_SHAPE ( 'NONE', 'NONE',  #18375 ) ;
#16740 = CARTESIAN_POINT ( 'NONE',  ( -0.05938372350920063936, 28.87819992234353705, 3.680117784833935701 ) ) ;
#16741 = DIRECTION ( 'NONE',  ( 0.000000000000000000, -0.000000000000000000, 1.000000000000000000 ) ) ;
#16742 = FACE_OUTER_BOUND ( 'NONE', #3313, .T. ) ;
#16743 = AXIS2_PLACEMENT_3D ( 'NONE', #10134, #7728, #3296 ) ;
#16744 = CARTESIAN_POINT ( 'NONE',  ( -5.330712181944245322E-15, -28.36584563134306691, -7.686165607253494514 ) ) ;
#16745 = AXIS2_PLACEMENT_3D ( 'NONE', #14923, #12380, #16485 ) ;
#16746 = FACE_OUTER_BOUND ( 'NONE', #2828, .T. ) ;
#16747 = APPLICATION_CONTEXT ( 'automotive_design' ) ;
#16748 = CARTESIAN_POINT ( 'NONE',  ( 8.000000000000001776, 18.79999999999999361, -2.500000000000002220 ) ) ;
#16749 = CARTESIAN_POINT ( 'NONE',  ( 0.000000000000000000, 36.39999999999999147, 2.500000000000000000 ) ) ;
#16750 = CARTESIAN_POINT ( 'NONE',  ( -2.121784821874996396, -19.35194882682896633, -9.763202243652322920 ) ) ;
#16751 = CARTESIAN_POINT ( 'NONE',  ( -3.706921591972381904E-14, -18.76849698692083379, -9.496498676479825818 ) ) ;
#16752 = DIRECTION ( 'NONE',  ( -0.000000000000000000, 1.000000000000000000, -0.000000000000000000 ) ) ;
#16753 = CARTESIAN_POINT ( 'NONE',  ( -1.989345975306426206, 35.24680007765648071, 1.515154207786343799 ) ) ;
#16754 = LINE ( 'NONE', #1078, #4372 ) ;
#16755 = CARTESIAN_POINT ( 'NONE',  ( 2.798362969681366330, 36.49680007765648071, -2.102939460078824929 ) ) ;
#16756 = FACE_OUTER_BOUND ( 'NONE', #59, .T. ) ;
#16757 = ADVANCED_FACE ( 'NONE', ( #14310 ), #9778, .F. ) ;
#16758 = DIRECTION ( 'NONE',  ( -6.162975822039154730E-33, 0.5735764363510414965, 0.8191520442889950182 ) ) ;
#16759 = ORIENTED_EDGE ( 'NONE', *, *, #2155, .T. ) ;
#16760 = CARTESIAN_POINT ( 'NONE',  ( 4.730628863548789710E-15, -17.11170270152969053, -8.699544261015072166 ) ) ;
#16761 = CARTESIAN_POINT ( 'NONE',  ( -2.864755990943265829, 23.24680007765647716, -2.011557305968488141 ) ) ;
#16762 = EDGE_CURVE ( 'NONE', #3421, #2215, #4565, .T. ) ;
#16763 = CARTESIAN_POINT ( 'NONE',  ( 2.199999999999999734, 0.000000000000000000, 0.000000000000000000 ) ) ;
#16764 = EDGE_CURVE ( 'NONE', #4547, #14275, #10206, .T. ) ;
#16765 = CARTESIAN_POINT ( 'NONE',  ( 2.121784821875004390, -23.52471740128279620, -15.72253336585475658 ) ) ;
#16766 = CARTESIAN_POINT ( 'NONE',  ( 12.00000000000000178, 48.00000000000000000, -15.00000000000000000 ) ) ;
#16767 = CARTESIAN_POINT ( 'NONE',  ( -3.999999999999997335, -20.56202776116204234, -9.110456801337205590 ) ) ;
#16768 = CARTESIAN_POINT ( 'NONE',  ( -8.500000000000005329, 0.000000000000000000, 20.49999999999999645 ) ) ;
#16769 = CARTESIAN_POINT ( 'NONE',  ( 4.730628863548789710E-15, -22.24162695414431212, -16.02583535712476959 ) ) ;
#16770 = EDGE_LOOP ( 'NONE', ( #12572, #12166 ) ) ;
#16771 = CARTESIAN_POINT ( 'NONE',  ( -4.000000000000004441, -25.33494834008745755, -7.874257998310924656 ) ) ;
#16772 = CARTESIAN_POINT ( 'NONE',  ( -4.000000000000004441, -23.59270991537611550, -5.386083664789867775 ) ) ;
#16773 = CARTESIAN_POINT ( 'NONE',  ( 0.05938372350926800214, 17.37180007765647716, 2.628655560595669183 ) ) ;
#16774 = ORIENTED_EDGE ( 'NONE', *, *, #13088, .F. ) ;
#16775 = CARTESIAN_POINT ( 'NONE',  ( -8.000000000000003553, 18.79999999999999361, -2.500000000000001776 ) ) ;
#16776 = CARTESIAN_POINT ( 'NONE',  ( 3.607379964056363075, 38.50319992234354771, 2.690724712371229010 ) ) ;
#16777 = UNCERTAINTY_MEASURE_WITH_UNIT (LENGTH_MEASURE( 1.000000000000000082E-05 ), #5096, 'distance_accuracy_value', 'NONE');
#16778 = DIRECTION ( 'NONE',  ( -0.000000000000000000, -1.000000000000000000, -0.000000000000000000 ) ) ;
#16779 = CARTESIAN_POINT ( 'NONE',  ( 0.8262555684460829442, 25.25319992234354771, -2.360188852285421302 ) ) ;
#16780 = AXIS2_PLACEMENT_3D ( 'NONE', #6872, #7047, #18036 ) ;
#16781 = ORIENTED_EDGE ( 'NONE', *, *, #18063, .F. ) ;
#16782 = CARTESIAN_POINT ( 'NONE',  ( 2.121784821874994176, -28.37330216599443489, -9.832559698173744422 ) ) ;
#16783 = CARTESIAN_POINT ( 'NONE',  ( -4.481649420246366589, 27.87180007765647716, 1.518615910253458878 ) ) ;
#16784 = AXIS2_PLACEMENT_3D ( 'NONE', #10222, #420, #14229 ) ;
#16785 = CARTESIAN_POINT ( 'NONE',  ( -4.243569643749997233, -24.23781626479742712, -14.60519903057256208 ) ) ;
#16786 = EDGE_CURVE ( 'NONE', #5987, #10898, #5684, .T. ) ;
#16787 = ORIENTED_EDGE ( 'NONE', *, *, #14842, .F. ) ;
#16788 = PLANE ( 'NONE',  #3551 ) ;
#16789 = ADVANCED_FACE ( 'NONE', ( #9938 ), #15607, .T. ) ;
#16790 = DIRECTION ( 'NONE',  ( 0.000000000000000000, 0.8191520442889952403, -0.5735764363510413855 ) ) ;
#16791 = VECTOR ( 'NONE', #8118, 1000.000000000000000 ) ;
#16792 = DIRECTION ( 'NONE',  ( -0.000000000000000000, 1.000000000000000000, -0.000000000000000000 ) ) ;
#16793 = CARTESIAN_POINT ( 'NONE',  ( -4.243569643749997233, -21.39861290485977463, -10.55039641134203521 ) ) ;
#16794 = ORIENTED_EDGE ( 'NONE', *, *, #13744, .T. ) ;
#16795 = CARTESIAN_POINT ( 'NONE',  ( 8.499999999999994671, 10.00000000000000000, 20.49999999999999645 ) ) ;
#16796 = ORIENTED_EDGE ( 'NONE', *, *, #5062, .T. ) ;
#16797 = CIRCLE ( 'NONE', #9944, 0.9999999999999991118 ) ;
#16798 = CARTESIAN_POINT ( 'NONE',  ( 1.999999999999994449, -27.82948002549519018, -9.423659499041770360 ) ) ;
#16799 = CARTESIAN_POINT ( 'NONE',  ( -8.000000000000001776, 43.00000000000000000, -2.499999999999997335 ) ) ;
#16800 = CARTESIAN_POINT ( 'NONE',  ( 3.518350579753631191, 16.87180007765647360, 1.080741659609802729 ) ) ;
#16801 = ORIENTED_EDGE ( 'NONE', *, *, #17359, .F. ) ;
#16802 = CARTESIAN_POINT ( 'NONE',  ( 0.05938372350920109732, 35.12819992234354771, -3.680117784833935701 ) ) ;
#16803 = CARTESIAN_POINT ( 'NONE',  ( -2.211161402132838738, 19.12819992234354061, 2.942372952327218183 ) ) ;
#16804 = CARTESIAN_POINT ( 'NONE',  ( -4.000000000000000888, -25.85221876035684474, -12.63931462504386793 ) ) ;
#16805 = CARTESIAN_POINT ( 'NONE',  ( 0.8262555684461332373, 27.24680007765648426, 2.360188852285403982 ) ) ;
#16806 = CARTESIAN_POINT ( 'NONE',  ( 4.518350579753602325, 25.62819992234354416, -1.405661355842793725 ) ) ;
#16807 = UNCERTAINTY_MEASURE_WITH_UNIT (LENGTH_MEASURE( 1.000000000000000082E-05 ), #1483, 'distance_accuracy_value', 'NONE');
#16808 = CARTESIAN_POINT ( 'NONE',  ( -3.999999999999997335, -22.62690293202579284, -12.05940416077758925 ) ) ;
#16809 =( BOUNDED_SURFACE ( )  B_SPLINE_SURFACE ( 3, 2, ( 
 ( #3592, #16126, #10814 ),
 ( #16489, #8029, #4977 ),
 ( #17805, #10632, #2303 ),
 ( #7658, #815, #2128 ),
 ( #16306, #3416, #13417 ),
 ( #14927, #13686, #17627 ),
 ( #1003, #3767, #6643 ),
 ( #12201, #641, #7757 ),
 ( #4888, #7847, #12109 ),
 ( #6551, #2220, #17889 ),
 ( #5160, #6280, #2397 ),
 ( #6460, #16212, #731 ),
 ( #9418, #5067, #15095 ),
 ( #14736, #10537, #7936 ),
 ( #10722, #12291, #9152 ),
 ( #17981, #13594, #6374 ) ),
 .UNSPECIFIED., .F., .F., .T. ) 
 B_SPLINE_SURFACE_WITH_KNOTS ( ( 4, 2, 2, 2, 2, 2, 2, 4 ),
 ( 3, 3 ),
 ( 0.000000000000000000, 0.004776775202955720404, 0.007165162804433580605, 0.009553550405911440807, 0.01194193800738930014, 0.01433032560886716121, 0.01671871321034502228, 0.01910710081182288161 ),
 ( 0.000000000000000000, 1.000000000000000000 ),
 .UNSPECIFIED. ) 
 GEOMETRIC_REPRESENTATION_ITEM ( )  RATIONAL_B_SPLINE_SURFACE ( (
 ( 1.000000000000000000, 0.8431867568967624793, 1.000000000000000000),
 ( 1.000000000000000000, 0.8377920060143945191, 1.000000000000000000),
 ( 1.000000000000000000, 0.8290876956143414800, 1.000000000000000000),
 ( 1.000000000000000000, 0.8092161897602034859, 1.000000000000000000),
 ( 1.000000000000000000, 0.8014575563008032866, 1.000000000000000000),
 ( 1.000000000000000000, 0.7833253045188315333, 1.000000000000000000),
 ( 1.000000000000000000, 0.7729073097594592046, 1.000000000000000000),
 ( 1.000000000000000000, 0.7492617761142137400, 1.000000000000000000),
 ( 1.000000000000000000, 0.7360775662804031061, 1.000000000000000000),
 ( 1.000000000000000000, 0.7066113664073706557, 1.000000000000000000),
 ( 1.000000000000000000, 0.6903329448040008698, 1.000000000000000000),
 ( 1.000000000000000000, 0.6541098336270502189, 1.000000000000000000),
 ( 1.000000000000000000, 0.6341722888203963349, 1.000000000000000000),
 ( 1.000000000000000000, 0.5897142078662076514, 1.000000000000000000),
 ( 1.000000000000000000, 0.5651944592878379581, 1.000000000000000000),
 ( 1.000000000000000000, 0.5376207706124462860, 1.000000000000000000) ) ) 
 REPRESENTATION_ITEM ( '' )  SURFACE ( )  );
#16810 = ORIENTED_EDGE ( 'NONE', *, *, #14316, .T. ) ;
#16811 = CARTESIAN_POINT ( 'NONE',  ( 2.121784821875004390, -17.10424616687832966, -6.553150170094818705 ) ) ;
#16812 = CARTESIAN_POINT ( 'NONE',  ( 2.864755990943265829, 19.49680007765648071, 2.011557305968487697 ) ) ;
#16813 = DIRECTION ( 'NONE',  ( 0.000000000000000000, 1.000000000000000000, 0.000000000000000000 ) ) ;
#16814 = CARTESIAN_POINT ( 'NONE',  ( 4.730628863548789710E-15, -19.14431419784868993, -11.60241431796419853 ) ) ;
#16815 = DIRECTION ( 'NONE',  ( -1.000000000000000000, 0.000000000000000000, 4.336808689942021680E-16 ) ) ;
#16816 = CARTESIAN_POINT ( 'NONE',  ( 2.000000000000004441, -18.13202342554876267, -7.653209906595630940 ) ) ;
#16817 = CARTESIAN_POINT ( 'NONE',  ( -14.99999999999999645, -4.000000000000000000, -30.00000000000000000 ) ) ;
#16818 = ORIENTED_EDGE ( 'NONE', *, *, #14766, .F. ) ;
#16819 = ORIENTED_EDGE ( 'NONE', *, *, #8970, .T. ) ;
#16820 = CARTESIAN_POINT ( 'NONE',  ( -2.211161402132902243, 18.37180007765647005, -2.942372952327172886 ) ) ;
#16821 = CARTESIAN_POINT ( 'NONE',  ( 8.499999999999992895, 15.00000000000000000, 18.29999999999999716 ) ) ;
#16822 = EDGE_CURVE ( 'NONE', #5386, #9839, #6333, .T. ) ;
#16823 = DIRECTION ( 'NONE',  ( -0.000000000000000000, -0.000000000000000000, -1.000000000000000000 ) ) ;
#16824 = CARTESIAN_POINT ( 'NONE',  ( 0.000000000000000000, 5.977523610840987267, 32.81826849749789687 ) ) ;
#16825 = ORIENTED_EDGE ( 'NONE', *, *, #11863, .T. ) ;
#16826 = AXIS2_PLACEMENT_3D ( 'NONE', #18127, #16728, #4003 ) ;
#16827 = CARTESIAN_POINT ( 'NONE',  ( -2.055738996568281518, 39.25319992234354771, 1.423772053676066962 ) ) ;
#16828 = EDGE_CURVE ( 'NONE', #5641, #9296, #15600, .T. ) ;
#16829 = AXIS2_PLACEMENT_3D ( 'NONE', #16768, #15545, #2932 ) ;
#16830 = CARTESIAN_POINT ( 'NONE',  ( 2.121784821875004390, -21.20173283406107956, -12.40496758648432518 ) ) ;
#16831 = CARTESIAN_POINT ( 'NONE',  ( 0.05938372350927906274, 34.87180007765645939, 3.680117784833935701 ) ) ;
#16832 = EDGE_CURVE ( 'NONE', #6613, #17767, #14232, .T. ) ;
#16833 = CARTESIAN_POINT ( 'NONE',  ( 3.518350579753605434, 28.12819992234354416, -1.080741659609877114 ) ) ;
#16834 = CARTESIAN_POINT ( 'NONE',  ( 1.475796370471763337E-14, -22.05939178977998694, -14.19638352958117267 ) ) ;
#16835 = CYLINDRICAL_SURFACE ( 'NONE', #5505, 0.9999999999999991118 ) ;
#16836 = ADVANCED_FACE ( 'NONE', ( #5026 ), #9190, .T. ) ;
#16837 = CARTESIAN_POINT ( 'NONE',  ( 2.121784821874994176, -27.59897397692052934, -8.726704438383601214 ) ) ;
#16838 = VECTOR ( 'NONE', #12271, 1000.000000000000000 ) ;
#16839 = FACE_OUTER_BOUND ( 'NONE', #13543, .T. ) ;
#16840 = DIRECTION ( 'NONE',  ( -3.373073425510457965E-16, 0.000000000000000000, -1.000000000000000000 ) ) ;
#16841 = DIRECTION ( 'NONE',  ( -0.000000000000000000, 1.000000000000000000, -0.000000000000000000 ) ) ;
#16842 = CARTESIAN_POINT ( 'NONE',  ( 2.121784821874994176, -24.98561633879609545, -4.994442936591867443 ) ) ;
#16843 = DIRECTION ( 'NONE',  ( -0.000000000000000000, -0.000000000000000000, -1.000000000000000000 ) ) ;
#16844 = CARTESIAN_POINT ( 'NONE',  ( 1.497042530366477164, 38.87180007765646650, -2.161531897785062384 ) ) ;
#16845 = DIRECTION ( 'NONE',  ( -1.000000000000000000, 0.000000000000000000, 4.336808689942021680E-16 ) ) ;
#16846 = CARTESIAN_POINT ( 'NONE',  ( 2.864755990943265829, 34.49680007765648071, 2.011557305968487697 ) ) ;
#16847 = CIRCLE ( 'NONE', #10291, 10.00000000000000178 ) ;
#16848 = CARTESIAN_POINT ( 'NONE',  ( -3.432133564730650122, 14.99999999999999822, -1.977182347542568941 ) ) ;
#16849 = AXIS2_PLACEMENT_3D ( 'NONE', #15888, #8917, #6046 ) ;
#16850 = EDGE_LOOP ( 'NONE', ( #7560, #3707 ) ) ;
#16851 = CARTESIAN_POINT ( 'NONE',  ( 2.121784821874994176, -24.75977061698287329, -4.671901819153075230 ) ) ;
#16852 = UNCERTAINTY_MEASURE_WITH_UNIT (LENGTH_MEASURE( 1.000000000000000082E-05 ), #3873, 'distance_accuracy_value', 'NONE');
#16853 = CARTESIAN_POINT ( 'NONE',  ( -2.115076519116362519, 32.62180007765646650, 3.012182706137107147 ) ) ;
#16854 = LINE ( 'NONE', #4305, #7663 ) ;
#16855 = CARTESIAN_POINT ( 'NONE',  ( 0.000000000000000000, 5.977523610840987267, 32.81826849749789687 ) ) ;
#16856 = DIRECTION ( 'NONE',  ( 0.000000000000000000, 0.000000000000000000, -1.000000000000000000 ) ) ;
#16857 = VECTOR ( 'NONE', #11794, 999.9999999999998863 ) ;
#16858 = FACE_OUTER_BOUND ( 'NONE', #15231, .T. ) ;
#16860 = DIRECTION ( 'NONE',  ( 0.5735764363510414965, -0.6710100716628397688, 0.4698463103929523821 ) ) ;
#16859 = AXIS2_PLACEMENT_3D ( 'NONE', #15770, #3351, #8702 ) ;
#16861 = CARTESIAN_POINT ( 'NONE',  ( -2.121784821875005722, -28.64216612053397526, -10.21653721893421363 ) ) ;
#16862 = ORIENTED_EDGE ( 'NONE', *, *, #11625, .F. ) ;
#16863 = CARTESIAN_POINT ( 'NONE',  ( 8.499999999999992895, 15.00000000000000000, 22.69999999999999929 ) ) ;
#16864 = CARTESIAN_POINT ( 'NONE',  ( -3.999999999999997335, -20.36844571459851139, -8.833992987396438679 ) ) ;
#16865 = CARTESIAN_POINT ( 'NONE',  ( 2.115076519116362963, 36.37180007765648782, -3.012182706137107147 ) ) ;
#16866 = ORIENTED_EDGE ( 'NONE', *, *, #4085, .T. ) ;
#16867 = CARTESIAN_POINT ( 'NONE',  ( -10.00000000000000178, 20.99999999999999289, -2.500000000000001776 ) ) ;
#16868 = CARTESIAN_POINT ( 'NONE',  ( 2.829195390882805583, 17.12180007765647716, 3.793023760679204770 ) ) ;
#16869 = CARTESIAN_POINT ( 'NONE',  ( -1.734723475976807094E-15, 16.59999999999999787, -2.500000000000000000 ) ) ;
#16870 = CARTESIAN_POINT ( 'NONE',  ( 0.05938372350921204690, 35.12819992234354771, -2.628655560595669183 ) ) ;
#16871 = EDGE_CURVE ( 'NONE', #6078, #15759, #2100, .T. ) ;
#16872 = ORIENTED_EDGE ( 'NONE', *, *, #15, .F. ) ;
#16873 = CARTESIAN_POINT ( 'NONE',  ( -2.121784821874996396, -22.22341586131136992, -13.86408216537410354 ) ) ;
#16874 = AXIS2_PLACEMENT_3D ( 'NONE', #2513, #8141, #13802 ) ;
#16875 = CARTESIAN_POINT ( 'NONE',  ( -4.518350579753632523, 33.12180007765647360, -1.405661355842698468 ) ) ;
#16876 = EDGE_LOOP ( 'NONE', ( #5734, #2291, #4539, #14509 ) ) ;
#16877 = CARTESIAN_POINT ( 'NONE',  ( 0.000000000000000000, 13.00000000000000178, 0.000000000000000000 ) ) ;
#16878 =( NAMED_UNIT ( * ) SI_UNIT ( $, .STERADIAN. ) SOLID_ANGLE_UNIT ( ) );
#16879 = DIRECTION ( 'NONE',  ( 0.000000000000000000, -1.000000000000000000, 0.000000000000000000 ) ) ;
#16880 = AXIS2_PLACEMENT_3D ( 'NONE', #12563, #6905, #18249 ) ;
#16881 = CARTESIAN_POINT ( 'NONE',  ( 8.499999999999994671, 15.00000000000000178, 22.64999999999999147 ) ) ;
#16882 = CIRCLE ( 'NONE', #12116, 0.5000000000000026645 ) ;
#16883 = CARTESIAN_POINT ( 'NONE',  ( 4.243569643750000786, -23.25499295915232167, -8.930091773994377036 ) ) ;
#16884 = EDGE_LOOP ( 'NONE', ( #10386, #8645, #16705, #9629 ) ) ;
#16885 = CIRCLE ( 'NONE', #9464, 0.9999999999999991118 ) ;
#16886 = DIRECTION ( 'NONE',  ( 0.000000000000000000, 0.000000000000000000, 1.000000000000000000 ) ) ;
#16887 =( GEOMETRIC_REPRESENTATION_CONTEXT ( 3 ) GLOBAL_UNCERTAINTY_ASSIGNED_CONTEXT ( ( #8402 ) ) GLOBAL_UNIT_ASSIGNED_CONTEXT ( ( #15835, #14066, #1559 ) ) REPRESENTATION_CONTEXT ( 'NONE', 'WORKASPACE' ) );
#16888 = VERTEX_POINT ( 'NONE', #7529 ) ;
#16889 = CARTESIAN_POINT ( 'NONE',  ( -3.999999999999997335, -22.69143028182022803, -12.15155876676686830 ) ) ;
#16890 = FACE_OUTER_BOUND ( 'NONE', #12640, .T. ) ;
#16891 = CARTESIAN_POINT ( 'NONE',  ( -4.000000000000000888, -25.78769141056240954, -12.54716001905459066 ) ) ;
#16892 = SURFACE_STYLE_USAGE ( .BOTH. , #11203 ) ;
#16893 = CARTESIAN_POINT ( 'NONE',  ( 4.518350579753602325, 20.62819992234354416, -1.405661355842793725 ) ) ;
#16894 = CARTESIAN_POINT ( 'NONE',  ( 3.481649420246395010, 18.37819992234354771, 1.193696214020467439 ) ) ;
#16895 = EDGE_CURVE ( 'NONE', #15867, #8360, #8589, .T. ) ;
#16896 = CARTESIAN_POINT ( 'NONE',  ( 4.000000000000000888, -25.72316406217786522, -12.45500541507884051 ) ) ;
#16897 = CARTESIAN_POINT ( 'NONE',  ( 2.481649420246374138, 34.12180007765647360, -0.8687765177876252132 ) ) ;
#16898 = CARTESIAN_POINT ( 'NONE',  ( -4.518350579753602325, 26.87819992234354416, 1.405661355842794391 ) ) ;
#16899 = CARTESIAN_POINT ( 'NONE',  ( 4.000000000000003553, -21.68050181204658244, -10.70780328770074696 ) ) ;
#16900 = EDGE_LOOP ( 'NONE', ( #7215, #13786 ) ) ;
#16901 = AXIS2_PLACEMENT_3D ( 'NONE', #14712, #3394, #14806 ) ;
#16902 = CARTESIAN_POINT ( 'NONE',  ( -2.121784821875005722, -23.51224186791935011, -2.890246122824515318 ) ) ;
#16903 = CARTESIAN_POINT ( 'NONE',  ( -3.500000000000000444, 22.99680007765647716, 0.05647727720536892260 ) ) ;
#16904 = CARTESIAN_POINT ( 'NONE',  ( -1.661723472263481630E-14, -20.57526276142661459, -12.07682761599016175 ) ) ;
#16905 = CARTESIAN_POINT ( 'NONE',  ( 2.121784821875004390, -20.16929524862920431, -10.93049390676413601 ) ) ;
#16906 = CARTESIAN_POINT ( 'NONE',  ( 0.000000000000000000, 43.00000000000000000, 0.000000000000000000 ) ) ;
#16907 = LINE ( 'NONE', #4183, #7172 ) ;
#16908 = LINE ( 'NONE', #9565, #5288 ) ;
#16909 = ORIENTED_EDGE ( 'NONE', *, *, #16016, .T. ) ;
#16910 = ORIENTED_EDGE ( 'NONE', *, *, #1795, .F. ) ;
#16911 = CARTESIAN_POINT ( 'NONE',  ( -3.481649420246369697, 25.37180007765648071, 1.193696214020542490 ) ) ;
#16912 = CARTESIAN_POINT ( 'NONE',  ( -2.000000000000005773, -24.71065815213145100, -4.969520257213599024 ) ) ;
#16913 = CARTESIAN_POINT ( 'NONE',  ( -5.577813053751546416E-15, -29.32240898478130120, -10.62147269458723464 ) ) ;
#16914 = CARTESIAN_POINT ( 'NONE',  ( -1.734723475976807094E-15, 27.59999999999999432, -2.500000000000000000 ) ) ;
#16915 = CARTESIAN_POINT ( 'NONE',  ( 3.999999999999996447, -24.79722043171331336, -7.106302957796752473 ) ) ;
#16916 = ORIENTED_EDGE ( 'NONE', *, *, #12720, .T. ) ;
#16917 = VECTOR ( 'NONE', #17581, 1000.000000000000000 ) ;
#16918 = CARTESIAN_POINT ( 'NONE',  ( -3.500000000000000444, 19.50319992234354416, -0.05647727720529563400 ) ) ;
#16919 = CARTESIAN_POINT ( 'NONE',  ( -2.121784821875005722, -26.06107215695429247, -6.530353019633736267 ) ) ;
#16920 = CARTESIAN_POINT ( 'NONE',  ( -1.027846397803541700, 34.99680007765648071, 3.346150245485522312 ) ) ;
#16921 =( BOUNDED_CURVE ( )  B_SPLINE_CURVE ( 1, ( #8121, #3952 ),
 .UNSPECIFIED., .F., .T. ) 
 B_SPLINE_CURVE_WITH_KNOTS ( ( 2, 2 ),
 ( 0.000000000000000000, 1.000000000000000000 ),
 .UNSPECIFIED. ) 
 CURVE ( )  GEOMETRIC_REPRESENTATION_ITEM ( )  RATIONAL_B_SPLINE_CURVE ( ( 0.9401540804572323662, 0.9401540804572323662 ) ) 
 REPRESENTATION_ITEM ( '' )  );
#16922 = CARTESIAN_POINT ( 'NONE',  ( -1.027846397803611866, 27.50319992234354771, -3.346150245485499219 ) ) ;
#16923 = CARTESIAN_POINT ( 'NONE',  ( 3.772879157352770907, -10.00000000000000178, -12.59063537424807677 ) ) ;
#16924 = DIRECTION ( 'NONE',  ( -0.000000000000000000, -0.5735764363510414965, -0.8191520442889950182 ) ) ;
#16925 = CARTESIAN_POINT ( 'NONE',  ( -4.243569643749997233, -22.17294109393367307, -11.65625167113217664 ) ) ;
#16926 = EDGE_CURVE ( 'NONE', #2439, #10092, #14217, .T. ) ;
#16927 = CIRCLE ( 'NONE', #16032, 10.00000000000000000 ) ;
#16928 = EDGE_CURVE ( 'NONE', #8838, #6628, #2240, .T. ) ;
#16929 = CARTESIAN_POINT ( 'NONE',  ( 5.810221930991194676E-16, -23.67257551772224033, -16.50024865515073458 ) ) ;
#16930 = DIRECTION ( 'NONE',  ( 0.000000000000000000, 0.8191520442889952403, -0.5735764363510413855 ) ) ;
#16931 = CARTESIAN_POINT ( 'NONE',  ( -2.000000000000005773, -23.74274791649401095, -3.587201183482685352 ) ) ;
#16932 = CARTESIAN_POINT ( 'NONE',  ( 4.730628863548789710E-15, -16.30511083791103744, -7.547611698733671659 ) ) ;
#16933 = CARTESIAN_POINT ( 'NONE',  ( -3.000000000000001332, 15.00000000000000355, 3.048632113068340848E-14 ) ) ;
#16934 = SURFACE_SIDE_STYLE ('',( #17109 ) ) ;
#16935 = EDGE_CURVE ( 'NONE', #6078, #15292, #1991, .T. ) ;
#16936 = ORIENTED_EDGE ( 'NONE', *, *, #3559, .F. ) ;
#16937 = CARTESIAN_POINT ( 'NONE',  ( -0.05938372350926768989, 38.62180007765647360, -2.628655560595669183 ) ) ;
#16938 = CARTESIAN_POINT ( 'NONE',  ( 2.121784821875004390, -24.04093619399873560, -16.45977020571485028 ) ) ;
#16939 = CARTESIAN_POINT ( 'NONE',  ( -3.500000000000000444, 35.49680007765648071, 0.05647727720536892260 ) ) ;
#16940 = AXIS2_PLACEMENT_3D ( 'NONE', #9024, #13557, #6428 ) ;
#16941 = CARTESIAN_POINT ( 'NONE',  ( -9.324442068587902810, -9.992495910828282035, -2.158041910186991874 ) ) ;
#16942 = ORIENTED_EDGE ( 'NONE', *, *, #16695, .F. ) ;
#16943 = CARTESIAN_POINT ( 'NONE',  ( 4.243569643750000786, -19.89957080649872623, -4.138052314903757356 ) ) ;
#16944 = CARTESIAN_POINT ( 'NONE',  ( 3.500000000000000444, 34.24680007765648071, -0.05647727720536935281 ) ) ;
#16945 = EDGE_CURVE ( 'NONE', #9963, #17338, #11884, .T. ) ;
#16946 = CARTESIAN_POINT ( 'NONE',  ( -2.121784821875005722, -29.93271310232382021, -12.05962931858445231 ) ) ;
#16947 = CYLINDRICAL_SURFACE ( 'NONE', #1988, 2.149999999999995470 ) ;
#16948 = COLOUR_RGB ( '',0.8941176470588234615, 0.8941176470588234615, 0.8941176470588234615 ) ;
#16949 = PLANE ( 'NONE',  #8862 ) ;
#16950 = DIRECTION ( 'NONE',  ( -0.000000000000000000, 1.000000000000000000, -0.000000000000000000 ) ) ;
#16951 = CARTESIAN_POINT ( 'NONE',  ( 4.730628863548789710E-15, -20.69297057599650813, -13.81412483754448495 ) ) ;
#16952 = ORIENTED_EDGE ( 'NONE', *, *, #8137, .T. ) ;
#16953 = CARTESIAN_POINT ( 'NONE',  ( 1.533898589781675205E-14, -26.93489706776514581, -7.211752309227528634 ) ) ;
#16954 = CARTESIAN_POINT ( 'NONE',  ( 2.000000000000004441, -17.42222258626929943, -6.639509252794765892 ) ) ;
#16955 = CARTESIAN_POINT ( 'NONE',  ( -1.989345975306426206, 17.74680007765647716, 1.515154207786343799 ) ) ;
#16956 = ORIENTED_EDGE ( 'NONE', *, *, #6652, .F. ) ;
#16957 = CARTESIAN_POINT ( 'NONE',  ( -3.999999999999997335, -20.36844571459851139, -8.833992987396436902 ) ) ;
#16958 = AXIS2_PLACEMENT_3D ( 'NONE', #4575, #7165, #15709 ) ;
#16959 =( LENGTH_UNIT ( ) NAMED_UNIT ( * ) SI_UNIT ( .MILLI., .METRE. ) );
#16960 = UNCERTAINTY_MEASURE_WITH_UNIT (LENGTH_MEASURE( 1.000000000000000082E-05 ), #13427, 'distance_accuracy_value', 'NONE');
#16961 = CIRCLE ( 'NONE', #6287, 0.9999999999999991118 ) ;
#16962 = CARTESIAN_POINT ( 'NONE',  ( -0.7188294034286550893, 37.50319992234354771, -2.395093729190349130 ) ) ;
#16963 = ORIENTED_EDGE ( 'NONE', *, *, #14072, .F. ) ;
#16964 = CARTESIAN_POINT ( 'NONE',  ( 4.243569643750003451, -23.54952454117618288, -13.62221657742576220 ) ) ;
#16965 = PRODUCT_DEFINITION_FORMATION_WITH_SPECIFIED_SOURCE ( 'ANY', '', #3977, .NOT_KNOWN. ) ;
#16966 = CARTESIAN_POINT ( 'NONE',  ( -3.673772985318219053, 35.74680007765646650, -2.599342558260952174 ) ) ;
#16967 = EDGE_CURVE ( 'NONE', #7588, #4253, #3643, .T. ) ;
#16968 = VERTEX_POINT ( 'NONE', #9289 ) ;
#16969 = SURFACE_STYLE_FILL_AREA ( #12674 ) ;
#16970 = PRESENTATION_STYLE_ASSIGNMENT (( #9890 ) ) ;
#16971 = VECTOR ( 'NONE', #3427, 1000.000000000000000 ) ;
#16972 = DIRECTION ( 'NONE',  ( 0.000000000000000000, 0.000000000000000000, 1.000000000000000000 ) ) ;
#16973 = TOROIDAL_SURFACE ( 'NONE', #13405, 2.200000000000000178, 0.2000000000000000111 ) ;
#16974 = CARTESIAN_POINT ( 'NONE',  ( 4.243569643750003451, -20.96843057759649653, -9.936032378125284836 ) ) ;
#16975 = ORIENTED_EDGE ( 'NONE', *, *, #1738, .T. ) ;
#16976 = ORIENTED_EDGE ( 'NONE', *, *, #3538, .F. ) ;
#16977 = DIRECTION ( 'NONE',  ( 3.469446951953612217E-16, -0.000000000000000000, 1.000000000000000000 ) ) ;
#16978 = ORIENTED_EDGE ( 'NONE', *, *, #14422, .F. ) ;
#16979 = CARTESIAN_POINT ( 'NONE',  ( -2.000000000000005773, -26.84006067278963670, -8.010622222643258183 ) ) ;
#16980 = CARTESIAN_POINT ( 'NONE',  ( 1.300000000000000044, 1.082531754730548856, -0.6250000000000002220 ) ) ;
#16981 =( NAMED_UNIT ( * ) PLANE_ANGLE_UNIT ( ) SI_UNIT ( $, .RADIAN. ) );
#16982 = CARTESIAN_POINT ( 'NONE',  ( 4.481649420246397675, 15.87819992234354061, 1.518615910253363177 ) ) ;
#16983 = CARTESIAN_POINT ( 'NONE',  ( 3.481649420246395010, 28.37819992234354416, 1.193696214020467439 ) ) ;
#16984 = CARTESIAN_POINT ( 'NONE',  ( 4.000000000000000888, -26.23938285489380462, -13.19224225493893599 ) ) ;
#16985 = CARTESIAN_POINT ( 'NONE',  ( -2.500000000000001332, 40.49680007765648071, 0.05647727720535858364 ) ) ;
#16986 = CIRCLE ( 'NONE', #14914, 2.999999999999999556 ) ;
#16987 = CARTESIAN_POINT ( 'NONE',  ( 4.481649420246397675, 33.37819992234354771, 1.518615910253363177 ) ) ;
#16988 = TOROIDAL_SURFACE ( 'NONE', #15500, 9.000000000000001776, 0.9999999999999991118 ) ;
#16989 = CARTESIAN_POINT ( 'NONE',  ( -3.999999999999997335, -21.33635595023594789, -10.21631206112735235 ) ) ;
#16990 = EDGE_LOOP ( 'NONE', ( #17743, #10666, #6004, #10258 ) ) ;
#16991 = ADVANCED_FACE ( 'NONE', ( #496 ), #4847, .F. ) ;
#16992 = DIRECTION ( 'NONE',  ( 0.000000000000000000, 0.000000000000000000, -1.000000000000000000 ) ) ;
#16993 = CARTESIAN_POINT ( 'NONE',  ( -3.481649420246369697, 25.37180007765648071, 1.193696214020542490 ) ) ;
#16994 = ADVANCED_FACE ( 'NONE', ( #10495 ), #16168, .F. ) ;
#16995 = CARTESIAN_POINT ( 'NONE',  ( 9.911006336631391633, -9.930557276593896532, 8.884713581541163308 ) ) ;
#16996 = CARTESIAN_POINT ( 'NONE',  ( 2.121784821875004390, -20.42740464498717401, -11.29911232669418197 ) ) ;
#16997 = EDGE_CURVE ( 'NONE', #317, #4607, #6703, .T. ) ;
#16998 = CARTESIAN_POINT ( 'NONE',  ( 1.336863392178479160, 26.24680007765647716, -4.297206761780677731 ) ) ;
#16999 = AXIS2_PLACEMENT_3D ( 'NONE', #8665, #7278, #347 ) ;
#17000 = DIRECTION ( 'NONE',  ( 0.000000000000000000, 0.000000000000000000, -1.000000000000000000 ) ) ;
#17001 = ADVANCED_FACE ( 'NONE', ( #16540 ), #1323, .T. ) ;
#17002 = FACE_OUTER_BOUND ( 'NONE', #15613, .T. ) ;
#17003 = ORIENTED_EDGE ( 'NONE', *, *, #477, .F. ) ;
#17004 = VERTEX_POINT ( 'NONE', #10772 ) ;
#17005 = CARTESIAN_POINT ( 'NONE',  ( 2.211161402132902243, 22.12180007765648071, 2.942372952327172442 ) ) ;
#17006 = DIRECTION ( 'NONE',  ( 1.000000000000000000, 0.000000000000000000, 0.000000000000000000 ) ) ;
#17007 = FILL_AREA_STYLE_COLOUR ( '', #13418 ) ;
#17008 = CARTESIAN_POINT ( 'NONE',  ( -1.999999999999996225, -21.70253674183399184, -12.75243138229462758 ) ) ;
#17009 = CARTESIAN_POINT ( 'NONE',  ( -4.000000000000000888, -26.88465634578871999, -14.11378830476406065 ) ) ;
#17010 = VERTEX_POINT ( 'NONE', #13830 ) ;
#17011 = CARTESIAN_POINT ( 'NONE',  ( 3.500000000000000444, 15.75319992234354416, 0.05647727720529520379 ) ) ;
#17012 = CARTESIAN_POINT ( 'NONE',  ( -4.243569643750005227, -25.33721873525807666, -7.632328254085517294 ) ) ;
#17013 = CARTESIAN_POINT ( 'NONE',  ( 0.05938372350927906274, 37.37180007765645939, 3.680117784833935701 ) ) ;
#17014 = CARTESIAN_POINT ( 'NONE',  ( 3.500000000000000444, 38.25319992234354061, 0.05647727720529520379 ) ) ;
#17015 = DIRECTION ( 'NONE',  ( -0.000000000000000000, -1.000000000000000000, -0.000000000000000000 ) ) ;
#17016 = CARTESIAN_POINT ( 'NONE',  ( 1.999999999999994449, -27.82948002549519018, -9.423659499041770360 ) ) ;
#17017 = VECTOR ( 'NONE', #17402, 1000.000000000000000 ) ;
#17018 = CARTESIAN_POINT ( 'NONE',  ( -4.243569643750005227, -24.07893542801298281, -5.835313456926535025 ) ) ;
#17019 = CARTESIAN_POINT ( 'NONE',  ( -14.99999999999999645, -4.000000000000000000, 30.00000000000000000 ) ) ;
#17020 = DIRECTION ( 'NONE',  ( -3.469446951953613696E-16, -0.000000000000000000, -1.000000000000000000 ) ) ;
#17021 = FACE_OUTER_BOUND ( 'NONE', #18091, .T. ) ;
#17022 =( BOUNDED_CURVE ( )  B_SPLINE_CURVE ( 2, ( #10336, #17614, #13211, #4592, #714, #15918, #3219, #14721, #9137 ),
 .UNSPECIFIED., .F., .T. ) 
 B_SPLINE_CURVE_WITH_KNOTS ( ( 3, 2, 2, 2, 3 ),
 ( 0.4051724137931034808, 0.4080459770114942541, 0.4137931034482758563, 0.4195402298850574585, 0.4224137931034482873 ),
 .UNSPECIFIED. ) 
 CURVE ( )  GEOMETRIC_REPRESENTATION_ITEM ( )  RATIONAL_B_SPLINE_CURVE ( ( 0.9330127018922194093, 0.9330127018922200755, 1.000000000000000000, 0.8660254037844387076, 1.000000000000000000, 0.8660254037844387076, 1.000000000000000000, 0.9330127018922187432, 0.9330127018922194093 ) ) 
 REPRESENTATION_ITEM ( '' )  );
#17023 = CARTESIAN_POINT ( 'NONE',  ( -4.243569643749997233, -18.78525526673533719, -6.818134909550300549 ) ) ;
#17024 = CARTESIAN_POINT ( 'NONE',  ( -2.607440925699020084, 15.00000000000000533, -1.613633664971267700 ) ) ;
#17025 = DIRECTION ( 'NONE',  ( 0.000000000000000000, 0.000000000000000000, 1.000000000000000000 ) ) ;
#17026 = ORIENTED_EDGE ( 'NONE', *, *, #1626, .T. ) ;
#17027 = CARTESIAN_POINT ( 'NONE',  ( 2.481649420246391902, 23.37819992234354771, 0.8687765177875720335 ) ) ;
#17028 = CARTESIAN_POINT ( 'NONE',  ( -4.243569643750005227, -28.95075028426964181, -12.79298613310618471 ) ) ;
#17029 = CARTESIAN_POINT ( 'NONE',  ( 8.500000000000001776, 14.80000000000000071, -18.29999999999999716 ) ) ;
#17030 = FACE_OUTER_BOUND ( 'NONE', #17426, .T. ) ;
#17031 = LINE ( 'NONE', #5697, #4916 ) ;
#17032 = EDGE_CURVE ( 'NONE', #8512, #15647, #8576, .T. ) ;
#17033 = ORIENTED_EDGE ( 'NONE', *, *, #16478, .F. ) ;
#17034 = CARTESIAN_POINT ( 'NONE',  ( 4.243569643749997233, -22.44424258441252817, -3.500730130702893295 ) ) ;
#17035 = CARTESIAN_POINT ( 'NONE',  ( -1.135272562821090014, 28.49680007765648071, -3.311245368580554072 ) ) ;
#17036 = CARTESIAN_POINT ( 'NONE',  ( -4.243569643750004339, -27.40209390612183071, -10.58127561352589829 ) ) ;
#17037 = CARTESIAN_POINT ( 'NONE',  ( -1.734723475976807094E-15, 27.59999999999999432, -2.500000000000000000 ) ) ;
#17038 = FACE_OUTER_BOUND ( 'NONE', #10440, .T. ) ;
#17039 = LINE ( 'NONE', #12566, #8218 ) ;
#17040 = CARTESIAN_POINT ( 'NONE',  ( -4.243569643749997233, -22.39878681574689523, -11.97879278857096885 ) ) ;
#17041 = EDGE_LOOP ( 'NONE', ( #13123, #14062, #4755, #4817 ) ) ;
#17042 = CARTESIAN_POINT ( 'NONE',  ( 3.579096709490575479E-14, -26.67678767140717966, -6.843133889297480899 ) ) ;
#17043 = CARTESIAN_POINT ( 'NONE',  ( -4.000000000000004441, -21.78594414087033471, -2.805754725279534956 ) ) ;
#17044 = CARTESIAN_POINT ( 'NONE',  ( 1.593127413382998903, 22.12180007765648071, 2.091722143975139669 ) ) ;
#17045 = ORIENTED_EDGE ( 'NONE', *, *, #13613, .F. ) ;
#17046 = DIRECTION ( 'NONE',  ( -3.469446951953613696E-16, -0.000000000000000000, -1.000000000000000000 ) ) ;
#17047 = EDGE_CURVE ( 'NONE', #8977, #1682, #13925, .T. ) ;
#17048 = CARTESIAN_POINT ( 'NONE',  ( -4.000000000000000888, -23.01301540041918869, -8.584512005813342839 ) ) ;
#17049 = EDGE_CURVE ( 'NONE', #1500, #12929, #10671, .T. ) ;
#17050 = CARTESIAN_POINT ( 'NONE',  ( -2.481649420246391902, 34.62819992234354771, -0.8687765177875723666 ) ) ;
#17051 = ORIENTED_EDGE ( 'NONE', *, *, #8774, .T. ) ;
#17052 = CARTESIAN_POINT ( 'NONE',  ( 2.121784821874994176, -27.59897397692052934, -8.726704438383601214 ) ) ;
#17053 = ADVANCED_FACE ( 'NONE', ( #5209 ), #6686, .T. ) ;
#17054 = CARTESIAN_POINT ( 'NONE',  ( -2.829195390882805139, 33.37180007765647360, -3.793023760679206102 ) ) ;
#17055 = ORIENTED_EDGE ( 'NONE', *, *, #4237, .F. ) ;
#17056 = DIRECTION ( 'NONE',  ( 0.000000000000000000, 1.000000000000000000, 0.000000000000000000 ) ) ;
#17057 = CARTESIAN_POINT ( 'NONE',  ( 4.299564228933482956E-15, -22.57561058249592278, -14.93362036944126814 ) ) ;
#17058 = DIRECTION ( 'NONE',  ( -1.000000000000000000, 0.000000000000000000, 0.000000000000000000 ) ) ;
#17059 = DIRECTION ( 'NONE',  ( 1.000000000000000000, 0.000000000000000000, 0.000000000000000000 ) ) ;
#17060 = CARTESIAN_POINT ( 'NONE',  ( 2.000000000000004441, -23.29421135270813537, -15.02557830519658388 ) ) ;
#17061 = CARTESIAN_POINT ( 'NONE',  ( 4.243569643749996345, -23.21857077348643017, -4.606585390493037835 ) ) ;
#17062 = ORIENTED_EDGE ( 'NONE', *, *, #2099, .F. ) ;
#17063 = LINE ( 'NONE', #1656, #10274 ) ;
#17064 = ORIENTED_EDGE ( 'NONE', *, *, #1516, .T. ) ;
#17065 = VERTEX_POINT ( 'NONE', #9563 ) ;
#17066 = FACE_OUTER_BOUND ( 'NONE', #15561, .T. ) ;
#17067 = CARTESIAN_POINT ( 'NONE',  ( -2.829195390882724315, 19.12819992234354416, 3.793023760679264722 ) ) ;
#17068 = CARTESIAN_POINT ( 'NONE',  ( 3.518350579753606322, 30.62819992234354061, -1.080741659609876892 ) ) ;
#17069 = CARTESIAN_POINT ( 'NONE',  ( -2.000000000000005773, -28.64682644729541749, -10.59095116215359234 ) ) ;
#17070 = AXIS2_PLACEMENT_3D ( 'NONE', #9151, #16305, #7477 ) ;
#17071 = CARTESIAN_POINT ( 'NONE',  ( -2.500000000000001332, 35.49680007765647360, 0.05647727720535858364 ) ) ;
#17072 = EDGE_LOOP ( 'NONE', ( #9807, #1236, #6559, #16593 ) ) ;
#17073 = CARTESIAN_POINT ( 'NONE',  ( -1.336863392178569088, 37.50319992234353350, -4.297206761780648421 ) ) ;
#17074 = CARTESIAN_POINT ( 'NONE',  ( -5.279047395330986450E-15, -26.92557132411310050, -6.119585135346799376 ) ) ;
#17075 = ORIENTED_EDGE ( 'NONE', *, *, #7260, .F. ) ;
#17076 = EDGE_CURVE ( 'NONE', #3912, #7076, #4752, .T. ) ;
#17077 = VECTOR ( 'NONE', #5340, 1000.000000000000000 ) ;
#17078 = DIRECTION ( 'NONE',  ( -1.000000000000000000, -0.000000000000000000, -0.000000000000000000 ) ) ;
#17079 = CARTESIAN_POINT ( 'NONE',  ( 1.027846397803542144, 21.24680007765647716, -3.346150245485522312 ) ) ;
#17080 = CARTESIAN_POINT ( 'NONE',  ( 9.000000000000005329, -10.00000000000000000, -3.713574246709344884 ) ) ;
#17081 = CARTESIAN_POINT ( 'NONE',  ( 2.121784821874994176, -25.50183513151203130, -5.731679776451962915 ) ) ;
#17082 = AXIS2_PLACEMENT_3D ( 'NONE', #2010, #11811, #13302 ) ;
#17083 = CARTESIAN_POINT ( 'NONE',  ( -2.829195390882805139, 33.37180007765647360, -3.793023760679206102 ) ) ;
#17084 = CARTESIAN_POINT ( 'NONE',  ( 2.199999999999999734, 1.999999999999999112, 0.000000000000000000 ) ) ;
#17085 = ORIENTED_EDGE ( 'NONE', *, *, #14248, .F. ) ;
#17086 = ORIENTED_EDGE ( 'NONE', *, *, #13924, .F. ) ;
#17087 = CARTESIAN_POINT ( 'NONE',  ( -2.798362969681365886, 22.74680007765648071, 2.102939460078824929 ) ) ;
#17088 = CARTESIAN_POINT ( 'NONE',  ( -2.343145750507621194, -3.999999999999994671, 25.54267522293723758 ) ) ;
#17089 = DIRECTION ( 'NONE',  ( 0.000000000000000000, 0.000000000000000000, -1.000000000000000000 ) ) ;
#17090 = DIRECTION ( 'NONE',  ( -1.000000000000000000, 0.000000000000000000, -0.000000000000000000 ) ) ;
#17091 = FACE_OUTER_BOUND ( 'NONE', #3825, .T. ) ;
#17092 = ORIENTED_EDGE ( 'NONE', *, *, #14422, .T. ) ;
#17093 = CARTESIAN_POINT ( 'NONE',  ( -2.115076519116425580, 22.37819992234353350, -3.012182706137062738 ) ) ;
#17094 = CARTESIAN_POINT ( 'NONE',  ( -4.243569643750000786, -22.31934639735467840, -7.593850001747957990 ) ) ;
#17095 = CARTESIAN_POINT ( 'NONE',  ( 2.115076519116362963, 38.87180007765645939, -3.012182706137107147 ) ) ;
#17096 = ADVANCED_FACE ( 'NONE', ( #15241 ), #8169, .T. ) ;
#17097 = CARTESIAN_POINT ( 'NONE',  ( -3.481649420246394122, 37.12819992234354771, -1.193696214020467883 ) ) ;
#17098 = CARTESIAN_POINT ( 'NONE',  ( -8.500000000000005329, 13.00000000000000000, -20.49999999999999645 ) ) ;
#17099 = VECTOR ( 'NONE', #17763, 1000.000000000000000 ) ;
#17100 = CARTESIAN_POINT ( 'NONE',  ( 8.000000000000001776, 23.19999999999999574, -2.500000000000002220 ) ) ;
#17101 = EDGE_CURVE ( 'NONE', #851, #15989, #2822, .T. ) ;
#17102 = CARTESIAN_POINT ( 'NONE',  ( 2.121784821875004390, -19.16912133774208016, -9.502097529535200593 ) ) ;
#17103 = CARTESIAN_POINT ( 'NONE',  ( 8.499999999999994671, 15.00000000000000178, 20.49999999999999645 ) ) ;
#17104 = DIRECTION ( 'NONE',  ( 0.000000000000000000, -0.000000000000000000, 1.000000000000000000 ) ) ;
#17105 = DIRECTION ( 'NONE',  ( 0.000000000000000000, 0.000000000000000000, 1.000000000000000000 ) ) ;
#17106 = VECTOR ( 'NONE', #7938, 1000.000000000000227 ) ;
#17107 = CARTESIAN_POINT ( 'NONE',  ( 4.243569643750003451, -18.35507293947206264, -6.203770876333551954 ) ) ;
#17108 = DIRECTION ( 'NONE',  ( -3.469446951953613696E-16, -0.000000000000000000, -1.000000000000000000 ) ) ;
#17109 = SURFACE_STYLE_FILL_AREA ( #15354 ) ;
#17110 = ORIENTED_EDGE ( 'NONE', *, *, #14072, .T. ) ;
#17111 = CARTESIAN_POINT ( 'NONE',  ( -0.8262555684460826111, 21.50319992234354771, 2.360188852285421302 ) ) ;
#17112 = DIRECTION ( 'NONE',  ( 0.000000000000000000, 0.000000000000000000, -1.000000000000000000 ) ) ;
#17113 = CARTESIAN_POINT ( 'NONE',  ( 2.798362969681366330, 18.99680007765648071, -2.102939460078824929 ) ) ;
#17114 = EDGE_CURVE ( 'NONE', #13741, #14997, #17811, .T. ) ;
#17115 = CARTESIAN_POINT ( 'NONE',  ( 0.000000000000000000, 5.977523610840987267, 32.81826849749789687 ) ) ;
#17116 = VERTEX_POINT ( 'NONE', #16638 ) ;
#17117 = CARTESIAN_POINT ( 'NONE',  ( -2.121784821874996396, -17.31933733050996338, -6.860332186703194779 ) ) ;
#17118 = CARTESIAN_POINT ( 'NONE',  ( 1.135272562821090458, 32.24680007765648071, 3.311245368580554072 ) ) ;
#17119 = CIRCLE ( 'NONE', #9106, 8.000000000000003553 ) ;
#17120 = CARTESIAN_POINT ( 'NONE',  ( 4.730628863548789710E-15, -22.79010942140500262, -16.80914949947612413 ) ) ;
#17121 = TOROIDAL_SURFACE ( 'NONE', #15055, 2.200000000000000178, 0.2000000000000000111 ) ;
#17122 = CARTESIAN_POINT ( 'NONE',  ( -1.734723475976807094E-15, 38.59999999999999432, -2.500000000000000000 ) ) ;
#17123 = CARTESIAN_POINT ( 'NONE',  ( 4.243569643749997233, -27.31605744066918007, -10.45840280688254431 ) ) ;
#17124 =( BOUNDED_CURVE ( )  B_SPLINE_CURVE ( 2, ( #2725, #12439, #6960, #14018, #1329, #4009, #16912, #12618, #5398 ),
 .UNSPECIFIED., .F., .T. ) 
 B_SPLINE_CURVE_WITH_KNOTS ( ( 3, 2, 2, 2, 3 ),
 ( 0.6982758620689655249, 0.7011494252873563537, 0.7068965517241379004, 0.7126436781609195581, 0.7155172413793103869 ),
 .UNSPECIFIED. ) 
 CURVE ( )  GEOMETRIC_REPRESENTATION_ITEM ( )  RATIONAL_B_SPLINE_CURVE ( ( 0.9330127018922194093, 0.9330127018922194093, 1.000000000000000000, 0.8660254037844387076, 1.000000000000000000, 0.8660254037844387076, 1.000000000000000000, 0.9330127018922180770, 0.9330127018922194093 ) ) 
 REPRESENTATION_ITEM ( '' )  );
#17125 = CARTESIAN_POINT ( 'NONE',  ( 0.000000000000000000, 5.977523610840987267, 32.81826849749789687 ) ) ;
#17126 = CARTESIAN_POINT ( 'NONE',  ( -5.577813053751546416E-15, -24.09569370782749331, -3.156949689997003095 ) ) ;
#17127 = FACE_OUTER_BOUND ( 'NONE', #7619, .T. ) ;
#17128 = CARTESIAN_POINT ( 'NONE',  ( -4.243569643749997233, -23.17311500482080433, -13.08464804836111206 ) ) ;
#17129 = DIRECTION ( 'NONE',  ( -0.000000000000000000, -1.000000000000000000, 1.502314598737159031E-16 ) ) ;
#17130 = CARTESIAN_POINT ( 'NONE',  ( -5.279047395330986450E-15, -23.89278591761191350, -1.788318702175504038 ) ) ;
#17131 = AXIS2_PLACEMENT_3D ( 'NONE', #15595, #15515, #2812 ) ;
#17132 = CARTESIAN_POINT ( 'NONE',  ( -0.8262555684461330152, 25.99680007765648071, -2.360188852285403982 ) ) ;
#17133 = CIRCLE ( 'NONE', #9108, 0.9999999999999991118 ) ;
#17134 = ORIENTED_EDGE ( 'NONE', *, *, #201, .F. ) ;
#17135 = CARTESIAN_POINT ( 'NONE',  ( 1.135272562821090458, 22.24680007765648071, 3.311245368580554072 ) ) ;
#17136 = DIRECTION ( 'NONE',  ( 1.000000000000000000, 0.000000000000000000, 0.000000000000000000 ) ) ;
#17137 = DIRECTION ( 'NONE',  ( 0.000000000000000000, 0.000000000000000000, 1.000000000000000000 ) ) ;
#17138 = CARTESIAN_POINT ( 'NONE',  ( 0.7188294034286553114, 38.75319992234354061, 2.395093729190349130 ) ) ;
#17139 = ORIENTED_EDGE ( 'NONE', *, *, #13200, .F. ) ;
#17140 = CARTESIAN_POINT ( 'NONE',  ( -4.243569643750000786, -23.64215705368926379, -9.483019403889452192 ) ) ;
#17141 = CARTESIAN_POINT ( 'NONE',  ( -1.336863392178478716, 37.49680007765647360, 4.297206761780677731 ) ) ;
#17142 = ORIENTED_EDGE ( 'NONE', *, *, #870, .F. ) ;
#17143 = CIRCLE ( 'NONE', #14479, 4.000000000000000888 ) ;
#17144 = FILL_AREA_STYLE ('',( #15483 ) ) ;
#17145 = VECTOR ( 'NONE', #10660, 1000.000000000000000 ) ;
#17146 = CARTESIAN_POINT ( 'NONE',  ( 2.000000000000004441, -17.16411318991132617, -6.270890832864717268 ) ) ;
#17147 = EDGE_CURVE ( 'NONE', #15136, #10922, #12249, .T. ) ;
#17148 = CARTESIAN_POINT ( 'NONE',  ( 4.000000000000000888, -21.27077697429796288, -6.096337670278750842 ) ) ;
#17149 = FACE_OUTER_BOUND ( 'NONE', #691, .T. ) ;
#17150 = ADVANCED_FACE ( 'NONE', ( #16727 ), #9647, .F. ) ;
#17151 = DIRECTION ( 'NONE',  ( 1.000000000000000000, 0.000000000000000000, -4.336808689942021680E-16 ) ) ;
#17152 = CARTESIAN_POINT ( 'NONE',  ( -2.121784821875005722, -23.77035126427731981, -3.258864542754563942 ) ) ;
#17153 = ORIENTED_EDGE ( 'NONE', *, *, #11927, .T. ) ;
#17154 = EDGE_CURVE ( 'NONE', #8879, #13448, #5998, .T. ) ;
#17155 = AXIS2_PLACEMENT_3D ( 'NONE', #9041, #16011, #14907 ) ;
#17156 = FACE_OUTER_BOUND ( 'NONE', #105, .T. ) ;
#17157 = ORIENTED_EDGE ( 'NONE', *, *, #11571, .F. ) ;
#17158 = ORIENTED_EDGE ( 'NONE', *, *, #8626, .F. ) ;
#17159 = CARTESIAN_POINT ( 'NONE',  ( 9.000000000000000000, 36.39999999999999147, -2.500000000000001332 ) ) ;
#17160 = PRESENTATION_STYLE_ASSIGNMENT (( #18201 ) ) ;
#17161 = EDGE_CURVE ( 'NONE', #14266, #4345, #10392, .T. ) ;
#17162 = CIRCLE ( 'NONE', #15077, 2.149999999999995470 ) ;
#17163 = CARTESIAN_POINT ( 'NONE',  ( -4.499999999999999112, 17.00319992234354416, -0.05647727720528529505 ) ) ;
#17164 = CARTESIAN_POINT ( 'NONE',  ( -3.500000000000000444, 32.00319992234354771, -0.05647727720529563400 ) ) ;
#17165 = CARTESIAN_POINT ( 'NONE',  ( 2.500000000000001332, 34.24680007765648071, -0.05647727720535888202 ) ) ;
#17166 = EDGE_LOOP ( 'NONE', ( #15858, #13094, #995, #17996 ) ) ;
#17167 = CARTESIAN_POINT ( 'NONE',  ( -1.336863392178569088, 32.50319992234354771, -4.297206761780648421 ) ) ;
#17168 = CARTESIAN_POINT ( 'NONE',  ( -2.000000000000005773, -25.74309573756332270, -6.443993936933789968 ) ) ;
#17169 = VERTEX_POINT ( 'NONE', #13231 ) ;
#17170 = ADVANCED_FACE ( 'NONE', ( #14551 ), #11392, .F. ) ;
#17171 = CIRCLE ( 'NONE', #16575, 8.000000000000001776 ) ;
#17172 = DIRECTION ( 'NONE',  ( 0.000000000000000000, 0.000000000000000000, 1.000000000000000000 ) ) ;
#17173 = AXIS2_PLACEMENT_3D ( 'NONE', #3936, #9586, #5419 ) ;
#17174 = CARTESIAN_POINT ( 'NONE',  ( -0.05938372350927861171, 31.12180007765647005, -3.680117784833935701 ) ) ;
#17175 = CARTESIAN_POINT ( 'NONE',  ( -6.772465634063925322, -14.05063737647557964, -1.433670420094913522 ) ) ;
#17176 = PRODUCT_RELATED_PRODUCT_CATEGORY ( 'part', '', ( #17623 ) ) ;
#17177 = VECTOR ( 'NONE', #14261, 1000.000000000000000 ) ;
#17178 = CARTESIAN_POINT ( 'NONE',  ( -4.243569643749998122, -19.81769285216720888, -8.292608589270493269 ) ) ;
#17179 = CIRCLE ( 'NONE', #276, 0.9999999999999991118 ) ;
#17180 = CARTESIAN_POINT ( 'NONE',  ( -1.336863392178478716, 34.99680007765647360, 4.297206761780677731 ) ) ;
#17181 = CARTESIAN_POINT ( 'NONE',  ( -8.500000000000005329, 0.000000000000000000, 22.50000000000000000 ) ) ;
#17182 = EDGE_LOOP ( 'NONE', ( #8037, #17492, #900, #12883, #360 ) ) ;
#17183 = ORIENTED_EDGE ( 'NONE', *, *, #17501, .T. ) ;
#17184 = CARTESIAN_POINT ( 'NONE',  ( 2.115076519116362963, 26.37180007765648071, -3.012182706137107147 ) ) ;
#17185 = LINE ( 'NONE', #8707, #15177 ) ;
#17186 = CARTESIAN_POINT ( 'NONE',  ( -8.500000000000010658, 10.00000000000000000, 18.34999999999999432 ) ) ;
#17187 = DIRECTION ( 'NONE',  ( -0.000000000000000000, -1.000000000000000000, -0.000000000000000000 ) ) ;
#17188 = ORIENTED_EDGE ( 'NONE', *, *, #15651, .T. ) ;
#17189 = CARTESIAN_POINT ( 'NONE',  ( -3.481649420246394122, 19.62819992234354416, -1.193696214020467883 ) ) ;
#17190 = CARTESIAN_POINT ( 'NONE',  ( -4.000000000000000888, -26.36843755307278414, -13.37655146490396341 ) ) ;
#17191 = CARTESIAN_POINT ( 'NONE',  ( 4.243569643749996345, -24.47685408073152402, -6.403600187652020992 ) ) ;
#17192 = CARTESIAN_POINT ( 'NONE',  ( -3.518350579753630747, 35.62180007765648782, -1.080741659609802729 ) ) ;
#17193 = VECTOR ( 'NONE', #6972, 1000.000000000000000 ) ;
#17194 = CARTESIAN_POINT ( 'NONE',  ( 2.798362969681409851, 36.00319992234354771, 2.102939460078764977 ) ) ;
#17195 = CARTESIAN_POINT ( 'NONE',  ( -3.999999999999997335, -19.33600812916663614, -7.359519307676247735 ) ) ;
#17196 = CARTESIAN_POINT ( 'NONE',  ( 13.00000000000000178, 15.00000000000000000, 16.00000000000000000 ) ) ;
#17197 = CARTESIAN_POINT ( 'NONE',  ( 4.730628863548789710E-15, -18.66035907967750163, -10.91125478059535681 ) ) ;
#17198 = DIRECTION ( 'NONE',  ( -1.000000000000000000, 0.000000000000000000, 0.000000000000000000 ) ) ;
#17199 = DIRECTION ( 'NONE',  ( 0.000000000000000000, 0.000000000000000000, 1.000000000000000000 ) ) ;
#17200 = AXIS2_PLACEMENT_3D ( 'NONE', #14969, #2266, #10404 ) ;
#17201 = LINE ( 'NONE', #13091, #5638 ) ;
#17202 =( GEOMETRIC_REPRESENTATION_CONTEXT ( 3 ) GLOBAL_UNCERTAINTY_ASSIGNED_CONTEXT ( ( #16597 ) ) GLOBAL_UNIT_ASSIGNED_CONTEXT ( ( #15648, #537, #4696 ) ) REPRESENTATION_CONTEXT ( 'NONE', 'WORKASPACE' ) );
#17203 = LINE ( 'NONE', #8725, #5273 ) ;
#17204 = CARTESIAN_POINT ( 'NONE',  ( 2.121784821875004390, -18.10442007776545736, -7.981546547323755014 ) ) ;
#17205 = DIRECTION ( 'NONE',  ( -0.000000000000000000, 1.000000000000000000, -0.000000000000000000 ) ) ;
#17206 =( NAMED_UNIT ( * ) PLANE_ANGLE_UNIT ( ) SI_UNIT ( $, .RADIAN. ) );
#17207 = ORIENTED_EDGE ( 'NONE', *, *, #3197, .T. ) ;
#17208 = CARTESIAN_POINT ( 'NONE',  ( 1.989345975306457071, 21.00319992234354771, 1.515154207786300500 ) ) ;
#17209 = CARTESIAN_POINT ( 'NONE',  ( -4.243569643750005227, -28.43453149155370241, -12.05574929324608924 ) ) ;
#17210 = LINE ( 'NONE', #3101, #4203 ) ;
#17211 = CARTESIAN_POINT ( 'NONE',  ( 2.733110507866247652, 18.87180007765647716, -3.862833514489153686 ) ) ;
#17212 = LINE ( 'NONE', #13104, #13133 ) ;
#17213 = CARTESIAN_POINT ( 'NONE',  ( 0.000000000000000000, 0.000000000000000000, 0.000000000000000000 ) ) ;
#17214 = ORIENTED_EDGE ( 'NONE', *, *, #6265, .F. ) ;
#17215 = CARTESIAN_POINT ( 'NONE',  ( -4.243569643749998122, -17.78508135584820948, -5.389738532321367792 ) ) ;
#17216 = AXIS2_PLACEMENT_3D ( 'NONE', #6465, #8125, #736 ) ;
#17217 = CARTESIAN_POINT ( 'NONE',  ( 3.481649420246369697, 31.62180007765647360, -1.193696214020541824 ) ) ;
#17218 = CARTESIAN_POINT ( 'NONE',  ( 2.121784821875004390, -23.81509047218551700, -16.13722908827605806 ) ) ;
#17219 = CARTESIAN_POINT ( 'NONE',  ( 1.533898589781675205E-14, -26.93489706776514581, -7.211752309227528634 ) ) ;
#17220 = CARTESIAN_POINT ( 'NONE',  ( 2.121784821874994176, -29.11536668052359289, -10.89233765547263211 ) ) ;
#17221 = CARTESIAN_POINT ( 'NONE',  ( 3.064180744904201337, 3.871363374536846536, 34.29301777163557574 ) ) ;
#17222 = CARTESIAN_POINT ( 'NONE',  ( 9.999999999999998224, 18.79999999999999361, -2.500000000000001776 ) ) ;
#17223 = EDGE_CURVE ( 'NONE', #1671, #12707, #7894, .T. ) ;
#17224 = DIRECTION ( 'NONE',  ( 0.000000000000000000, 0.000000000000000000, -1.000000000000000000 ) ) ;
#17225 = CARTESIAN_POINT ( 'NONE',  ( -4.243569643750005227, -27.14398450976385746, -10.21265719359585233 ) ) ;
#17226 = CARTESIAN_POINT ( 'NONE',  ( 1.820000000000000062, 4.653657836759941744E-16, -3.799999999999999378 ) ) ;
#17227 = CARTESIAN_POINT ( 'NONE',  ( -4.000000000000004441, -22.56027232994424025, -3.911609985069676387 ) ) ;
#17228 = VECTOR ( 'NONE', #9225, 1000.000000000000000 ) ;
#17229 = CARTESIAN_POINT ( 'NONE',  ( -2.500000000000001332, 20.49680007765648071, 0.05647727720535858364 ) ) ;
#17230 = ORIENTED_EDGE ( 'NONE', *, *, #664, .T. ) ;
#17231 = CARTESIAN_POINT ( 'NONE',  ( -2.798362969681365886, 25.24680007765647716, 2.102939460078824929 ) ) ;
#17232 = CARTESIAN_POINT ( 'NONE',  ( -1.071796769724496334, -20.56373606070777882, -12.06036578133424264 ) ) ;
#17233 = SURFACE_SIDE_STYLE ('',( #8951 ) ) ;
#17234 = CARTESIAN_POINT ( 'NONE',  ( 0.000000000000000000, 34.19999999999999574, 2.500000000000000000 ) ) ;
#17235 = CARTESIAN_POINT ( 'NONE',  ( 2.500000000000001332, 35.75319992234354061, 0.05647727720530566764 ) ) ;
#17236 = ORIENTED_EDGE ( 'NONE', *, *, #7729, .F. ) ;
#17237 = CARTESIAN_POINT ( 'NONE',  ( -4.243569643750004339, -25.88570120251876361, -8.415642396436870953 ) ) ;
#17238 = CARTESIAN_POINT ( 'NONE',  ( 4.481649420246366589, 31.62180007765647716, -1.518615910253458212 ) ) ;
#17239 = AXIS2_PLACEMENT_3D ( 'NONE', #16547, #16450, #4010 ) ;
#17240 = ORIENTED_EDGE ( 'NONE', *, *, #15547, .T. ) ;
#17241 = PRESENTATION_LAYER_ASSIGNMENT (  '', '', ( #15169 ) ) ;
#17242 = SURFACE_STYLE_USAGE ( .BOTH. , #11453 ) ;
#17243 = CARTESIAN_POINT ( 'NONE',  ( 13.00000000000000178, 15.00000000000000178, -16.00000000000000000 ) ) ;
#17244 = CARTESIAN_POINT ( 'NONE',  ( -2.121784821874996396, -22.73963465402730577, -14.60131900523419901 ) ) ;
#17245 = CARTESIAN_POINT ( 'NONE',  ( 2.000000000000004441, -18.39013282190673237, -8.021828326525680453 ) ) ;
#17246 = DIRECTION ( 'NONE',  ( -0.000000000000000000, 1.000000000000000000, -0.000000000000000000 ) ) ;
#17247 = CARTESIAN_POINT ( 'NONE',  ( 0.000000000000000000, 3.000000000000000000, 0.000000000000000000 ) ) ;
#17248 = CARTESIAN_POINT ( 'NONE',  ( -5.330712181944245322E-15, -25.26853287504744472, -3.262744568092923014 ) ) ;
#17249 = ORIENTED_EDGE ( 'NONE', *, *, #17898, .F. ) ;
#17250 = AXIS2_PLACEMENT_3D ( 'NONE', #17308, #221, #1618 ) ;
#17251 = CARTESIAN_POINT ( 'NONE',  ( 3.276608177155980961, -25.09847727441901455, -15.56286022430290039 ) ) ;
#17252 = AXIS2_PLACEMENT_3D ( 'NONE', #12888, #8530, #1686 ) ;
#17253 = CARTESIAN_POINT ( 'NONE',  ( -8.000000000000003553, 31.99999999999999289, -2.500000000000001776 ) ) ;
#17254 = ORIENTED_EDGE ( 'NONE', *, *, #483, .T. ) ;
#17255 = VERTEX_POINT ( 'NONE', #14740 ) ;
#17256 = CYLINDRICAL_SURFACE ( 'NONE', #10729, 4.000000000000000000 ) ;
#17257 = MECHANICAL_DESIGN_GEOMETRIC_PRESENTATION_REPRESENTATION (  '', ( #12197 ), #11907 ) ;
#17258 = CARTESIAN_POINT ( 'NONE',  ( 4.518350579753602325, 18.12819992234354416, -1.405661355842793725 ) ) ;
#17259 = CARTESIAN_POINT ( 'NONE',  ( -3.481649420246394566, 29.62819992234354061, -1.193696214020467883 ) ) ;
#17260 = CARTESIAN_POINT ( 'NONE',  ( -1.593127413382998459, 38.37180007765647360, -2.091722143975139669 ) ) ;
#17261 = ADVANCED_FACE ( 'NONE', ( #4706 ), #2888, .F. ) ;
#17262 = ORIENTED_EDGE ( 'NONE', *, *, #8240, .T. ) ;
#17263 = CARTESIAN_POINT ( 'NONE',  ( -1.444289557195956863, 36.50319992234354061, 4.262301884875733471 ) ) ;
#17264 = CARTESIAN_POINT ( 'NONE',  ( 4.000000000000000888, -22.81943335244577398, -8.308048189859038146 ) ) ;
#17265 = ORIENTED_EDGE ( 'NONE', *, *, #15775, .T. ) ;
#17266 = CONICAL_SURFACE ( 'NONE', #18158, 2.000000000000001776, 1.029744260000000189 ) ;
#17267 = CARTESIAN_POINT ( 'NONE',  ( 0.000000000000000000, 9.254131787996968228, 30.52396275209373044 ) ) ;
#17268 = VECTOR ( 'NONE', #3145, 1000.000000000000000 ) ;
#17269 = CARTESIAN_POINT ( 'NONE',  ( -0.05938372350927861171, 33.62180007765648071, -3.680117784833935701 ) ) ;
#17270 = CARTESIAN_POINT ( 'NONE',  ( -7.143653376925515275, -13.70104873486882902, 0.6914076786229403915 ) ) ;
#17271 = CARTESIAN_POINT ( 'NONE',  ( -4.243569643750000786, -21.80312760463873900, -6.856613161887861629 ) ) ;
#17272 = CARTESIAN_POINT ( 'NONE',  ( -3.607379964056306676, 27.74680007765648071, 2.690724712371306282 ) ) ;
#17273 = PLANE ( 'NONE',  #18049 ) ;
#17274 = VERTEX_POINT ( 'NONE', #9828 ) ;
#17275 = ORIENTED_EDGE ( 'NONE', *, *, #17147, .F. ) ;
#17276 = CARTESIAN_POINT ( 'NONE',  ( 2.798362969681366330, 28.99680007765647716, -2.102939460078824929 ) ) ;
#17277 = DIRECTION ( 'NONE',  ( 0.000000000000000000, 0.000000000000000000, -1.000000000000000000 ) ) ;
#17278 = CIRCLE ( 'NONE', #14838, 2.149999999999995470 ) ;
#17279 = FILL_AREA_STYLE ('',( #6961 ) ) ;
#17280 = AXIS2_PLACEMENT_3D ( 'NONE', #16869, #16778, #12484 ) ;
#17281 = CARTESIAN_POINT ( 'NONE',  ( -9.184850993605147944E-16, 46.00000000000000000, -2.500000000000000000 ) ) ;
#17282 = CARTESIAN_POINT ( 'NONE',  ( 3.885274725274725949, -4.336808689942017736E-16, 0.000000000000000000 ) ) ;
#17283 = EDGE_LOOP ( 'NONE', ( #14743, #6541, #15762, #7168, #1976 ) ) ;
#17284 = AXIS2_PLACEMENT_3D ( 'NONE', #4897, #2045, #8781 ) ;
#17285 = CARTESIAN_POINT ( 'NONE',  ( 2.211161402132839626, 22.87819992234354416, -2.942372952327218183 ) ) ;
#17286 = DIRECTION ( 'NONE',  ( -1.000000000000000000, 0.000000000000000000, 0.000000000000000000 ) ) ;
#17287 = CARTESIAN_POINT ( 'NONE',  ( 4.243569643750003451, -20.67805750669378284, -9.521336655703981577 ) ) ;
#17288 = CARTESIAN_POINT ( 'NONE',  ( -2.211161402132902243, 35.87180007765648782, -2.942372952327172886 ) ) ;
#17289 = EDGE_CURVE ( 'NONE', #5876, #13013, #18100, .T. ) ;
#17290 = ADVANCED_FACE ( 'NONE', ( #2803 ), #3570, .T. ) ;
#17291 = CARTESIAN_POINT ( 'NONE',  ( -3.500000000000000444, 37.00319992234354061, -0.05647727720529563400 ) ) ;
#17292 = CARTESIAN_POINT ( 'NONE',  ( -2.121784821874996396, -24.03018163581715072, -16.44441110488443769 ) ) ;
#17293 = EDGE_CURVE ( 'NONE', #4992, #13832, #5756, .T. ) ;
#17294 = CARTESIAN_POINT ( 'NONE',  ( -2.000000000000005773, -29.87284607929082370, -12.34188865581455374 ) ) ;
#17295 = CARTESIAN_POINT ( 'NONE',  ( 4.243569643750003451, -20.96843057759649653, -9.936032378125284836 ) ) ;
#17296 = FACE_OUTER_BOUND ( 'NONE', #666, .T. ) ;
#17297 = AXIS2_PLACEMENT_3D ( 'NONE', #4031, #6813, #16476 ) ;
#17298 = AXIS2_PLACEMENT_3D ( 'NONE', #759, #6219, #17656 ) ;
#17299 = CARTESIAN_POINT ( 'NONE',  ( -6.660876705454564117, -10.00000000000000178, -8.457461752748960393 ) ) ;
#17300 = CARTESIAN_POINT ( 'NONE',  ( 8.500000000000019540, 10.00000000000000000, -20.49999999999998934 ) ) ;
#17301 = CARTESIAN_POINT ( 'NONE',  ( 8.500000000000001776, 14.99364916731036956, -20.49999999999999645 ) ) ;
#17302 = EDGE_LOOP ( 'NONE', ( #13145, #1914, #10592, #10926 ) ) ;
#17303 = CARTESIAN_POINT ( 'NONE',  ( -5.330712181944245322E-15, -24.46194101142878807, -2.110812005811521619 ) ) ;
#17304 = CARTESIAN_POINT ( 'NONE',  ( -1.055125536766255978, 15.00000000000066436, -3.294876966330904544 ) ) ;
#17305 = SURFACE_SIDE_STYLE ('',( #4477 ) ) ;
#17306 = EDGE_LOOP ( 'NONE', ( #16640, #11352, #14223, #16220 ) ) ;
#17307 = CARTESIAN_POINT ( 'NONE',  ( 1.989345975306457071, 23.50319992234355126, 1.515154207786300500 ) ) ;
#17308 = CARTESIAN_POINT ( 'NONE',  ( -8.500000000000010658, 14.80000000000000071, 22.69999999999999218 ) ) ;
#17309 = CIRCLE ( 'NONE', #4858, 0.2000000000000000944 ) ;
#17310 = CARTESIAN_POINT ( 'NONE',  ( 4.000000000000000000, 3.518949890710770134, -4.119968255444916849E-15 ) ) ;
#17311 = PLANE ( 'NONE',  #15296 ) ;
#17312 = VERTEX_POINT ( 'NONE', #14101 ) ;
#17313 = CARTESIAN_POINT ( 'NONE',  ( -2.211161402132902243, 38.37180007765648071, -2.942372952327172886 ) ) ;
#17314 = CARTESIAN_POINT ( 'NONE',  ( -2.121784821875005722, -29.19064858779466221, -10.99985136128556462 ) ) ;
#17315 = VECTOR ( 'NONE', #11957, 1000.000000000000000 ) ;
#17316 = EDGE_CURVE ( 'NONE', #9984, #8381, #9791, .T. ) ;
#17317 = PLANE ( 'NONE',  #11647 ) ;
#17318 = CARTESIAN_POINT ( 'NONE',  ( 4.243569643750003451, -24.03347965934736763, -14.31337611479460037 ) ) ;
#17319 = DIRECTION ( 'NONE',  ( 0.000000000000000000, 0.5735764363510414965, 0.8191520442889950182 ) ) ;
#17320 = SPHERICAL_SURFACE ( 'NONE', #11241, 4.324969328314201000 ) ;
#17321 = CARTESIAN_POINT ( 'NONE',  ( -8.500000000000005329, 0.000000000000000000, 20.49999999999999645 ) ) ;
#17322 = CARTESIAN_POINT ( 'NONE',  ( 4.243569643750000786, -25.02949505911335137, -11.46434341101345389 ) ) ;
#17323 = CARTESIAN_POINT ( 'NONE',  ( 4.299564228933482956E-15, -18.51038759056286054, -9.127880256549779858 ) ) ;
#17324 = CARTESIAN_POINT ( 'NONE',  ( 4.000000000000000888, -20.04475734230255668, -4.345400176617791210 ) ) ;
#17325 = CARTESIAN_POINT ( 'NONE',  ( -1.989345975306426206, 22.74680007765647716, 1.515154207786343799 ) ) ;
#17326 = TOROIDAL_SURFACE ( 'NONE', #17910, 9.000000000000003553, 0.9999999999999991118 ) ;
#17327 = EDGE_LOOP ( 'NONE', ( #2778, #13928 ) ) ;
#17328 = CARTESIAN_POINT ( 'NONE',  ( -1.135272562821090014, 20.99680007765647716, -3.311245368580554072 ) ) ;
#17329 = CARTESIAN_POINT ( 'NONE',  ( 9.000000000000001776, 16.59999999999999787, -2.500000000000002665 ) ) ;
#17330 = DIRECTION ( 'NONE',  ( 1.000000000000000000, 0.000000000000000000, 0.000000000000000000 ) ) ;
#17331 = LINE ( 'NONE', #4414, #2192 ) ;
#17332 = CARTESIAN_POINT ( 'NONE',  ( 2.864755990943222308, 18.00319992234354771, -2.011557305968548093 ) ) ;
#17333 = EDGE_CURVE ( 'NONE', #15033, #5353, #17407, .T. ) ;
#17334 = ORIENTED_EDGE ( 'NONE', *, *, #2747, .F. ) ;
#17335 = CARTESIAN_POINT ( 'NONE',  ( 4.243569643750000786, -23.51310235551028782, -9.298710193924424772 ) ) ;
#17336 = CARTESIAN_POINT ( 'NONE',  ( 2.798362969681366330, 16.49680007765647716, -2.102939460078824929 ) ) ;
#17337 = EDGE_CURVE ( 'NONE', #6382, #9005, #3327, .T. ) ;
#17338 = VERTEX_POINT ( 'NONE', #16587 ) ;
#17339 =( GEOMETRIC_REPRESENTATION_CONTEXT ( 3 ) GLOBAL_UNCERTAINTY_ASSIGNED_CONTEXT ( ( #1372 ) ) GLOBAL_UNIT_ASSIGNED_CONTEXT ( ( #11257, #2838, #9952 ) ) REPRESENTATION_CONTEXT ( 'NONE', 'WORKASPACE' ) );
#17340 = CARTESIAN_POINT ( 'NONE',  ( -5.577813053751546416E-15, -24.87002189690140241, -4.262804949787145858 ) ) ;
#17341 = CARTESIAN_POINT ( 'NONE',  ( 3.579096709490575479E-14, -25.70887743576973605, -5.460814815566567226 ) ) ;
#17342 = CARTESIAN_POINT ( 'NONE',  ( 4.243569643750000786, -25.31986813001606862, -11.87903913343475892 ) ) ;
#17343 = CARTESIAN_POINT ( 'NONE',  ( 3.999999999999996447, -23.18403670377106707, -4.802437832227187897 ) ) ;
#17344 = DIRECTION ( 'NONE',  ( 0.000000000000000000, 0.000000000000000000, 1.000000000000000000 ) ) ;
#17345 = CARTESIAN_POINT ( 'NONE',  ( 1.071796769724495224, -19.23171513056116666, -10.15804274500656312 ) ) ;
#17346 = CARTESIAN_POINT ( 'NONE',  ( -2.121784821874996396, -17.83555612322590278, -7.597569026563290251 ) ) ;
#17347 = ORIENTED_EDGE ( 'NONE', *, *, #14184, .F. ) ;
#17348 = CARTESIAN_POINT ( 'NONE',  ( -13.00000000000000178, 49.00000000000000000, 16.00000000000000000 ) ) ;
#17349 = DIRECTION ( 'NONE',  ( -0.000000000000000000, 1.000000000000000000, -0.000000000000000000 ) ) ;
#17350 = DIRECTION ( 'NONE',  ( -0.000000000000000000, -0.5735764363510414965, -0.8191520442889950182 ) ) ;
#17351 = EDGE_LOOP ( 'NONE', ( #3692, #2352, #708, #17214 ) ) ;
#17352 = ORIENTED_EDGE ( 'NONE', *, *, #2817, .T. ) ;
#17353 = DIRECTION ( 'NONE',  ( 0.000000000000000000, 0.8191520442889952403, -0.5735764363510413855 ) ) ;
#17354 = CARTESIAN_POINT ( 'NONE',  ( -1.336863392178569088, 30.00319992234354416, -4.297206761780648421 ) ) ;
#17355 = CARTESIAN_POINT ( 'NONE',  ( -0.05938372350920064630, 28.87819992234354061, 3.680117784833935701 ) ) ;
#17356 = CARTESIAN_POINT ( 'NONE',  ( 2.055738996568281518, 23.00319992234354771, -1.423772053676066518 ) ) ;
#17357 = VERTEX_POINT ( 'NONE', #2495 ) ;
#17358 = CARTESIAN_POINT ( 'NONE',  ( 1.444289557195957086, 35.25319992234354771, -4.262301884875733471 ) ) ;
#17359 = EDGE_CURVE ( 'NONE', #14942, #9017, #16637, .T. ) ;
#17360 = CARTESIAN_POINT ( 'NONE',  ( 4.000000000000000888, -22.04510516337187198, -7.202192930068894938 ) ) ;
#17361 = ORIENTED_EDGE ( 'NONE', *, *, #6478, .T. ) ;
#17362 = DIRECTION ( 'NONE',  ( -1.000000000000000000, 0.000000000000000000, 4.336808689942021680E-16 ) ) ;
#17363 = CARTESIAN_POINT ( 'NONE',  ( -2.864755990943265829, 28.24680007765648071, -2.011557305968488141 ) ) ;
#17364 = CARTESIAN_POINT ( 'NONE',  ( 9.356317142028521161, -10.00000000000000000, 13.59402740589572645 ) ) ;
#17365 = CARTESIAN_POINT ( 'NONE',  ( -5.330712181944246111E-15, -25.75248799321863657, -3.953904105461760743 ) ) ;
#17366 = VECTOR ( 'NONE', #13084, 1000.000000000000000 ) ;
#17367 = CARTESIAN_POINT ( 'NONE',  ( 3.607379964056306676, 33.99680007765647360, -2.690724712371305838 ) ) ;
#17368 = DIRECTION ( 'NONE',  ( 0.000000000000000000, 1.000000000000000000, 0.000000000000000000 ) ) ;
#17369 = VERTEX_POINT ( 'NONE', #4892 ) ;
#17370 = CARTESIAN_POINT ( 'NONE',  ( -2.211161402132902243, 30.87180007765647716, -2.942372952327172886 ) ) ;
#17371 = CARTESIAN_POINT ( 'NONE',  ( 0.000000000000000000, 9.254131787996968228, 30.52396275209373044 ) ) ;
#17372 = CARTESIAN_POINT ( 'NONE',  ( -12.99999999999999822, 48.00000000000000000, 0.000000000000000000 ) ) ;
#17373 = DIRECTION ( 'NONE',  ( 0.000000000000000000, 0.000000000000000000, 1.000000000000000000 ) ) ;
#17374 = EDGE_LOOP ( 'NONE', ( #11657, #6469, #2944 ) ) ;
#17375 = CARTESIAN_POINT ( 'NONE',  ( -3.518350579753605434, 29.37819992234354416, 1.080741659609877781 ) ) ;
#17376 = CARTESIAN_POINT ( 'NONE',  ( 2.200000000000000178, 0.000000000000000000, 0.000000000000000000 ) ) ;
#17377 = CARTESIAN_POINT ( 'NONE',  ( -2.121784821874996396, -19.09383943047100018, -9.394583823722271632 ) ) ;
#17378 = CARTESIAN_POINT ( 'NONE',  ( 2.864755990943265829, 36.99680007765648071, 2.011557305968487697 ) ) ;
#17379 = CARTESIAN_POINT ( 'NONE',  ( 2.864755990943222308, 38.00319992234354061, -2.011557305968548093 ) ) ;
#17380 = CARTESIAN_POINT ( 'NONE',  ( -2.121784821874996396, -23.77207223945918457, -16.07579268495438996 ) ) ;
#17381 = CARTESIAN_POINT ( 'NONE',  ( 4.713407268011036227E-15, -23.10115511886391104, -16.76302438318209553 ) ) ;
#17382 = CARTESIAN_POINT ( 'NONE',  ( 2.121784821874994176, -26.05031759877271469, -6.514993918803313910 ) ) ;
#17383 = CIRCLE ( 'NONE', #474, 0.9999999999999991118 ) ;
#17384 = DIRECTION ( 'NONE',  ( -0.000000000000000000, -0.5735764363510414965, -0.8191520442889950182 ) ) ;
#17385 = CARTESIAN_POINT ( 'NONE',  ( -7.003832385457668508, -10.00000000000000178, -7.945690313592825404 ) ) ;
#17386 = EDGE_CURVE ( 'NONE', #11658, #1682, #2708, .T. ) ;
#17387 = DIRECTION ( 'NONE',  ( 0.000000000000000000, 0.000000000000000000, 1.000000000000000000 ) ) ;
#17388 = EDGE_CURVE ( 'NONE', #17537, #4808, #9157, .T. ) ;
#17389 = DIRECTION ( 'NONE',  ( -0.7071067811865484609, 8.659560562354921765E-17, -0.7071067811865465735 ) ) ;
#17390 = ORIENTED_EDGE ( 'NONE', *, *, #7437, .T. ) ;
#17391 = ORIENTED_EDGE ( 'NONE', *, *, #1677, .F. ) ;
#17392 = CARTESIAN_POINT ( 'NONE',  ( -2.121784821874996396, -16.77085486324927999, -6.077018044351843784 ) ) ;
#17393 = LINE ( 'NONE', #3285, #12483 ) ;
#17394 = CARTESIAN_POINT ( 'NONE',  ( 4.000000000000000888, -20.56097613501849608, -5.082637016477885794 ) ) ;
#17395 = ADVANCED_FACE ( 'NONE', ( #8034 ), #13422, .T. ) ;
#17396 = ORIENTED_EDGE ( 'NONE', *, *, #7152, .F. ) ;
#17397 = CARTESIAN_POINT ( 'NONE',  ( -1.989345975306457071, 19.75319992234354771, -1.515154207786300944 ) ) ;
#17398 = CIRCLE ( 'NONE', #15306, 8.000000000000003553 ) ;
#17399 = CARTESIAN_POINT ( 'NONE',  ( -4.243569643749997233, -23.43122440117877048, -13.45326646829115980 ) ) ;
#17400 = CARTESIAN_POINT ( 'NONE',  ( -15.00000000000000178, 13.00000000000000178, -25.00000000000000355 ) ) ;
#17401 = EDGE_CURVE ( 'NONE', #13289, #14065, #930, .T. ) ;
#17402 = DIRECTION ( 'NONE',  ( -1.000000000000000000, -0.000000000000000000, -0.000000000000000000 ) ) ;
#17403 = CARTESIAN_POINT ( 'NONE',  ( 0.000000000000000000, 5.977523610840987267, 32.81826849749789687 ) ) ;
#17404 = ORIENTED_EDGE ( 'NONE', *, *, #13789, .T. ) ;
#17405 = CARTESIAN_POINT ( 'NONE',  ( 3.481649420246369697, 39.12180007765646650, -1.193696214020541824 ) ) ;
#17406 = CARTESIAN_POINT ( 'NONE',  ( -5.330712181944245322E-15, -30.94693959492275681, -11.37234980655397010 ) ) ;
#17407 =( BOUNDED_CURVE ( )  B_SPLINE_CURVE ( 2, ( #10, #101, #15939, #11742, #16036 ),
 .UNSPECIFIED., .F., .T. ) 
 B_SPLINE_CURVE_WITH_KNOTS ( ( 3, 2, 3 ),
 ( 0.9913793103448276245, 0.9942528735632183423, 0.9961881922148684287 ),
 .UNSPECIFIED. ) 
 CURVE ( )  GEOMETRIC_REPRESENTATION_ITEM ( )  RATIONAL_B_SPLINE_CURVE ( ( 0.9330127018922194093, 0.9330127018922206306, 1.000000000000000000, 0.9548846649268323272, 0.9401540970596700131 ) ) 
 REPRESENTATION_ITEM ( '' )  );
#17408 = EDGE_CURVE ( 'NONE', #3333, #12967, #9513, .T. ) ;
#17409 = DIRECTION ( 'NONE',  ( 0.000000000000000000, -0.9936001553129346631, -0.1129545544106654864 ) ) ;
#17410 = CARTESIAN_POINT ( 'NONE',  ( -2.121784821874996396, -22.70737097948255823, -14.55524170274294171 ) ) ;
#17411 = DIRECTION ( 'NONE',  ( 0.000000000000000000, 0.8191520442889952403, -0.5735764363510413855 ) ) ;
#17412 = CARTESIAN_POINT ( 'NONE',  ( -1.071796769724486564, -27.78527930735232232, -8.426224009662862002 ) ) ;
#17413 = CYLINDRICAL_SURFACE ( 'NONE', #10879, 4.000000000000000000 ) ;
#17414 = CARTESIAN_POINT ( 'NONE',  ( -4.243569643750000786, -23.60989337914451625, -9.436942101398194893 ) ) ;
#17415 = CARTESIAN_POINT ( 'NONE',  ( -1.734723475976807094E-15, 38.59999999999999432, -2.500000000000000000 ) ) ;
#17416 = CARTESIAN_POINT ( 'NONE',  ( 1.999999999999994449, -22.40918270197784778, -1.682672680510768792 ) ) ;
#17417 = CARTESIAN_POINT ( 'NONE',  ( -1.989345975306426206, 20.24680007765648071, 1.515154207786343799 ) ) ;
#17418 = ORIENTED_EDGE ( 'NONE', *, *, #10397, .F. ) ;
#17419 = CARTESIAN_POINT ( 'NONE',  ( -3.500000000000000444, 17.99680007765647716, 0.05647727720536892260 ) ) ;
#17420 = DIRECTION ( 'NONE',  ( 3.469446951953612217E-16, -0.000000000000000000, 1.000000000000000000 ) ) ;
#17421 = CARTESIAN_POINT ( 'NONE',  ( 0.000000000000000000, 0.000000000000000000, 0.000000000000000000 ) ) ;
#17422 = CARTESIAN_POINT ( 'NONE',  ( -5.279047395330986450E-15, -29.31308324112925945, -9.529305520706506272 ) ) ;
#17423 = DIRECTION ( 'NONE',  ( 0.000000000000000000, 0.000000000000000000, 1.000000000000000000 ) ) ;
#17424 = VECTOR ( 'NONE', #1275, 1000.000000000000000 ) ;
#17425 = CARTESIAN_POINT ( 'NONE',  ( -1.135272562821019626, 16.50319992234354416, 3.311245368580577164 ) ) ;
#17426 = EDGE_LOOP ( 'NONE', ( #15659, #1211, #600, #6141, #9749, #4138 ) ) ;
#17427 = CARTESIAN_POINT ( 'NONE',  ( 2.121784821875004390, -20.97588711224786095, -12.08242646904553474 ) ) ;
#17428 = CARTESIAN_POINT ( 'NONE',  ( 1.027846397803542144, 18.74680007765648071, -3.346150245485522312 ) ) ;
#17429 = ORIENTED_EDGE ( 'NONE', *, *, #1700, .F. ) ;
#17430 = CARTESIAN_POINT ( 'NONE',  ( -8.500000000000010658, 15.00000000000000000, 20.49999999999998934 ) ) ;
#17431 = CARTESIAN_POINT ( 'NONE',  ( -8.500000000000005329, 0.000000000000000000, -22.50000000000000000 ) ) ;
#17432 = CARTESIAN_POINT ( 'NONE',  ( 4.243569643749996345, -27.34832111521392761, -10.50448010937380161 ) ) ;
#17433 = CARTESIAN_POINT ( 'NONE',  ( 0.000000000000000000, 4.653657836759941744E-16, -3.799999999999999378 ) ) ;
#17434=STYLED_ITEM('',(#18396),#14214);
#17435 = CARTESIAN_POINT ( 'NONE',  ( -8.500000000000005329, 10.00000000000000000, -18.49999999999999645 ) ) ;
#17437 = CARTESIAN_POINT ( 'NONE',  ( 1.071796769724494780, -26.98789771684074168, -7.287445080560893018 ) ) ;
#17436 = VECTOR ( 'NONE', #9488, 1000.000000000000000 ) ;
#17438 = CARTESIAN_POINT ( 'NONE',  ( 2.121784821875004390, -18.13668375231020846, -8.027623849815011425 ) ) ;
#17439 = ORIENTED_EDGE ( 'NONE', *, *, #10397, .T. ) ;
#17440 = CARTESIAN_POINT ( 'NONE',  ( 1.533898589781675205E-14, -26.74131502120161841, -6.935288495286759058 ) ) ;
#17441 = PLANE ( 'NONE',  #8649 ) ;
#17442 = DIRECTION ( 'NONE',  ( -0.000000000000000000, -0.5735764363510414965, -0.8191520442889950182 ) ) ;
#17443 = EDGE_LOOP ( 'NONE', ( #17822, #11839, #10640 ) ) ;
#17444 = ORIENTED_EDGE ( 'NONE', *, *, #11927, .F. ) ;
#17445 = CYLINDRICAL_SURFACE ( 'NONE', #1868, 4.000000000000000000 ) ;
#17446 = CARTESIAN_POINT ( 'NONE',  ( 8.500000000000001776, 13.00000000000000000, -18.34999999999999787 ) ) ;
#17447 = CARTESIAN_POINT ( 'NONE',  ( 3.607379964056363075, 26.00319992234354771, 2.690724712371229010 ) ) ;
#17448 = CARTESIAN_POINT ( 'NONE',  ( 3.500000000000000444, 35.75319992234354771, 0.05647727720529520379 ) ) ;
#17449 = CARTESIAN_POINT ( 'NONE',  ( 2.500000000000001332, 18.25319992234354771, 0.05647727720530566764 ) ) ;
#17450 = ORIENTED_EDGE ( 'NONE', *, *, #13056, .T. ) ;
#17451 = COLOUR_RGB ( '',0.8941176470588234615, 0.8941176470588234615, 0.8941176470588234615 ) ;
#17452 = CARTESIAN_POINT ( 'NONE',  ( -1.444289557195956863, 39.00319992234354061, 4.262301884875733471 ) ) ;
#17453 = AXIS2_PLACEMENT_3D ( 'NONE', #7064, #34, #11328 ) ;
#17454 = CARTESIAN_POINT ( 'NONE',  ( 2.000000000000004441, -19.68067980369657377, -9.864920426175917356 ) ) ;
#17455 = ORIENTED_EDGE ( 'NONE', *, *, #12426, .T. ) ;
#17456 = DIRECTION ( 'NONE',  ( 0.000000000000000000, 0.000000000000000000, -1.000000000000000000 ) ) ;
#17457 = CARTESIAN_POINT ( 'NONE',  ( -2.211161402132902243, 28.37180007765647716, -2.942372952327172886 ) ) ;
#17458 = CARTESIAN_POINT ( 'NONE',  ( 0.000000000000000000, 9.254131787996968228, 30.52396275209373044 ) ) ;
#17459 = CARTESIAN_POINT ( 'NONE',  ( -4.243569643749998122, -19.04336466309330689, -7.186753329480350061 ) ) ;
#17460 = CARTESIAN_POINT ( 'NONE',  ( -2.733110507866247652, 32.62180007765647360, 3.862833514489154574 ) ) ;
#17461 = PRODUCT_DEFINITION_SHAPE ( 'NONE', 'NONE',  #2334 ) ;
#17462 = CARTESIAN_POINT ( 'NONE',  ( -1.734723475976807094E-15, 40.79999999999999716, -10.50000000000000178 ) ) ;
#17463 = EDGE_CURVE ( 'NONE', #1083, #16110, #2132, .T. ) ;
#17464 = ORIENTED_EDGE ( 'NONE', *, *, #7037, .F. ) ;
#17465 = CARTESIAN_POINT ( 'NONE',  ( -2.798362969681365886, 32.74680007765648071, 2.102939460078824929 ) ) ;
#17466 = CARTESIAN_POINT ( 'NONE',  ( 6.681132651088302232, -10.00000000000000178, 19.92483346546711687 ) ) ;
#17467 = DIRECTION ( 'NONE',  ( -0.000000000000000000, -1.000000000000000000, -0.000000000000000000 ) ) ;
#17468 = DIRECTION ( 'NONE',  ( 0.000000000000000000, 1.000000000000000000, 0.000000000000000000 ) ) ;
#17469 = DIRECTION ( 'NONE',  ( 0.000000000000000000, 0.000000000000000000, -1.000000000000000000 ) ) ;
#17470 = VERTEX_POINT ( 'NONE', #7942 ) ;
#17471 = CARTESIAN_POINT ( 'NONE',  ( 1.027846397803612311, 26.25319992234354771, 3.346150245485499219 ) ) ;
#17472 = CARTESIAN_POINT ( 'NONE',  ( -3.999999999999997335, -24.49819605632600883, -14.73188770627719890 ) ) ;
#17473 = CARTESIAN_POINT ( 'NONE',  ( -2.121784821874996396, -17.80329244868115168, -7.551491724072033840 ) ) ;
#17474 = CARTESIAN_POINT ( 'NONE',  ( -0.8262555684461330152, 20.99680007765648071, -2.360188852285403982 ) ) ;
#17475 = CARTESIAN_POINT ( 'NONE',  ( -2.829195390882724315, 19.12819992234354416, 3.793023760679264722 ) ) ;
#17476 = CARTESIAN_POINT ( 'NONE',  ( 4.243569643750000786, -27.12663390452184942, -14.45936807294509308 ) ) ;
#17477 = VECTOR ( 'NONE', #2110, 1000.000000000000000 ) ;
#17478 = CARTESIAN_POINT ( 'NONE',  ( 2.000000000000004441, -23.29421135270813537, -15.02557830519658388 ) ) ;
#17479 = CIRCLE ( 'NONE', #10030, 10.00000000000000000 ) ;
#17480 = CARTESIAN_POINT ( 'NONE',  ( 4.243569643749996345, -23.47668016984439632, -4.975203810423082906 ) ) ;
#17481 = AXIS2_PLACEMENT_3D ( 'NONE', #16326, #9261, #17823 ) ;
#17482 = CARTESIAN_POINT ( 'NONE',  ( -4.000000000000003553, 6.938893903907228378E-15, 24.28148006742132026 ) ) ;
#17483 = DIRECTION ( 'NONE',  ( 0.000000000000000000, 0.000000000000000000, 1.000000000000000000 ) ) ;
#17484 = DIRECTION ( 'NONE',  ( -0.000000000000000000, -0.5735764363510414965, -0.8191520442889950182 ) ) ;
#17485 = VECTOR ( 'NONE', #8728, 1000.000000000000000 ) ;
#17486 = FACE_OUTER_BOUND ( 'NONE', #9819, .T. ) ;
#17487 = ORIENTED_EDGE ( 'NONE', *, *, #17577, .T. ) ;
#17488 = ORIENTED_EDGE ( 'NONE', *, *, #17337, .F. ) ;
#17489 = DIRECTION ( 'NONE',  ( -0.000000000000000000, 1.000000000000000000, -0.000000000000000000 ) ) ;
#17490 = CARTESIAN_POINT ( 'NONE',  ( 1.071796769724485232, -28.98824553791006764, -10.14423783401199586 ) ) ;
#17491 = CARTESIAN_POINT ( 'NONE',  ( 1.999999999999994449, -23.44162028740971948, -3.157146360230959292 ) ) ;
#17492 = ORIENTED_EDGE ( 'NONE', *, *, #5322, .F. ) ;
#17493 = VECTOR ( 'NONE', #8471, 1000.000000000000000 ) ;
#17494 = CARTESIAN_POINT ( 'NONE',  ( 2.481649420246391902, 25.87819992234355126, 0.8687765177875720335 ) ) ;
#17495 = PRESENTATION_LAYER_ASSIGNMENT (  '', '', ( #6507 ) ) ;
#17496 = CARTESIAN_POINT ( 'NONE',  ( 4.730628863548789710E-15, -21.46729876507041013, -14.91998009733462816 ) ) ;
#17497 = CARTESIAN_POINT ( 'NONE',  ( -0.05938372350927861171, 21.12180007765648071, -3.680117784833935701 ) ) ;
#17498 = DIRECTION ( 'NONE',  ( 3.469446951953616161E-16, -0.000000000000000000, 1.000000000000000000 ) ) ;
#17499 = CARTESIAN_POINT ( 'NONE',  ( 4.778136680858137808, -10.00000000000000000, -10.60429372729831243 ) ) ;
#17500 = ADVANCED_FACE ( 'NONE', ( #12023 ), #14932, .F. ) ;
#17501 = EDGE_CURVE ( 'NONE', #1278, #5475, #327, .T. ) ;
#17502 = CARTESIAN_POINT ( 'NONE',  ( -1.027846397803541700, 37.49680007765647360, 3.346150245485522312 ) ) ;
#17503 = CARTESIAN_POINT ( 'NONE',  ( 4.243569643750003451, -23.80763393753414903, -13.99083499735581171 ) ) ;
#17504 = VECTOR ( 'NONE', #3468, 1000.000000000000000 ) ;
#17505 = EDGE_CURVE ( 'NONE', #1787, #4661, #13505, .T. ) ;
#17506 = AXIS2_PLACEMENT_3D ( 'NONE', #2648, #12634, #10882 ) ;
#17507 = PRESENTATION_STYLE_ASSIGNMENT (( #11808 ) ) ;
#17508 = CARTESIAN_POINT ( 'NONE',  ( -2.121784821874996396, -21.93304279040865623, -13.44938644295279850 ) ) ;
#17509 = DIRECTION ( 'NONE',  ( 0.000000000000000000, 0.000000000000000000, -1.000000000000000000 ) ) ;
#17510 = CARTESIAN_POINT ( 'NONE',  ( -3.999999999999997335, -18.30357054373476799, -5.885045627956057679 ) ) ;
#17511 = DIRECTION ( 'NONE',  ( 0.000000000000000000, 0.000000000000000000, 1.000000000000000000 ) ) ;
#17512 = CARTESIAN_POINT ( 'NONE',  ( 4.243569643750003451, -21.71049509212565454, -10.99581033542417252 ) ) ;
#17513 = CARTESIAN_POINT ( 'NONE',  ( 9.000000000000005329, 27.59999999999999432, 2.499999999999997335 ) ) ;
#17514 = CARTESIAN_POINT ( 'NONE',  ( 15.00000000000000355, 10.00000000000000000, 30.00000000000000000 ) ) ;
#17515 = CARTESIAN_POINT ( 'NONE',  ( 2.500000000000001332, 29.24680007765648071, -0.05647727720535888202 ) ) ;
#17516 = EDGE_LOOP ( 'NONE', ( #11855, #15894, #15298, #1490 ) ) ;
#17517 = CARTESIAN_POINT ( 'NONE',  ( 1.027846397803542144, 18.74680007765648071, -3.346150245485522312 ) ) ;
#17518 = CARTESIAN_POINT ( 'NONE',  ( 3.999999999999996447, -26.34587680986112801, -9.318013477377039777 ) ) ;
#17519 = DIRECTION ( 'NONE',  ( 1.000000000000000000, 0.000000000000000000, 0.000000000000000000 ) ) ;
#17520 = CIRCLE ( 'NONE', #5926, 2.000000000000001776 ) ;
#17521 = CARTESIAN_POINT ( 'NONE',  ( -2.000000000000005773, -28.13060765457947809, -9.853714322293496863 ) ) ;
#17522 = FACE_OUTER_BOUND ( 'NONE', #832, .T. ) ;
#17523 = CARTESIAN_POINT ( 'NONE',  ( -3.500000000000000444, 17.00319992234354416, -0.05647727720529563400 ) ) ;
#17524 =( BOUNDED_CURVE ( )  B_SPLINE_CURVE ( 2, ( #16451, #13469, #12256, #2183, #16270, #18038, #7993, #6692, #3561 ),
 .UNSPECIFIED., .F., .T. ) 
 B_SPLINE_CURVE_WITH_KNOTS ( ( 3, 2, 2, 2, 3 ),
 ( 0.1637931034482758563, 0.1666666666666666574, 0.1724137931034482873, 0.1781609195402298895, 0.1810344827586206906 ),
 .UNSPECIFIED. ) 
 CURVE ( )  GEOMETRIC_REPRESENTATION_ITEM ( )  RATIONAL_B_SPLINE_CURVE ( ( 0.9330127018922194093, 0.9330127018922194093, 1.000000000000000000, 0.8660254037844387076, 1.000000000000000000, 0.8660254037844387076, 1.000000000000000000, 0.9330127018922194093, 0.9330127018922194093 ) ) 
 REPRESENTATION_ITEM ( '' )  );
#17525 = ORIENTED_EDGE ( 'NONE', *, *, #12319, .T. ) ;
#17526 = CARTESIAN_POINT ( 'NONE',  ( -4.243569643750004339, -25.36948240980282421, -7.678405556576772817 ) ) ;
#17527 = CARTESIAN_POINT ( 'NONE',  ( -1.027846397803541700, 19.99680007765648071, 3.346150245485522312 ) ) ;
#17528 = EDGE_CURVE ( 'NONE', #5839, #9649, #820, .T. ) ;
#17529 = ORIENTED_EDGE ( 'NONE', *, *, #1984, .F. ) ;
#17530 = FACE_OUTER_BOUND ( 'NONE', #10483, .T. ) ;
#17531 = DIRECTION ( 'NONE',  ( -4.915049848600951133E-16, 0.000000000000000000, -1.000000000000000000 ) ) ;
#17532 = CARTESIAN_POINT ( 'NONE',  ( -4.243569643750005227, -27.43435758066657471, -10.62735291601715382 ) ) ;
#17533 = AXIS2_PLACEMENT_3D ( 'NONE', #9131, #2200, #16193 ) ;
#17534 = CARTESIAN_POINT ( 'NONE',  ( -1.734723475976807094E-15, 27.59999999999999432, -2.500000000000000000 ) ) ;
#17535 = CARTESIAN_POINT ( 'NONE',  ( 1.533898589781675205E-14, -26.99942441755958811, -7.303906915216807683 ) ) ;
#17536 = CARTESIAN_POINT ( 'NONE',  ( 2.769793372871041104, -22.38185876178289746, -1.928163851144596430 ) ) ;
#17537 = VERTEX_POINT ( 'NONE', #2308 ) ;
#17538 = CARTESIAN_POINT ( 'NONE',  ( 2.000000000000004441, -20.77764473892288777, -11.43154871188538557 ) ) ;
#17539 = CARTESIAN_POINT ( 'NONE',  ( 1.475796370471763337E-14, -21.86580974321645598, -13.91991971564040220 ) ) ;
#17540 = ORIENTED_EDGE ( 'NONE', *, *, #11117, .T. ) ;
#17541 = VERTEX_POINT ( 'NONE', #17809 ) ;
#17542 = CARTESIAN_POINT ( 'NONE',  ( 4.299564228933482956E-15, -20.83337215778458074, -12.44544603592020771 ) ) ;
#17543 = CARTESIAN_POINT ( 'NONE',  ( 7.999999999999998224, 46.00000000000000000, -2.500000000000003109 ) ) ;
#17544 = CARTESIAN_POINT ( 'NONE',  ( 0.05938372350919016857, 25.12819992234354416, -4.731580009072201776 ) ) ;
#17545 = EDGE_CURVE ( 'NONE', #7045, #17369, #1518, .T. ) ;
#17546 = CARTESIAN_POINT ( 'NONE',  ( 1.027846397803612311, 33.75319992234354771, 3.346150245485499219 ) ) ;
#17547 = CARTESIAN_POINT ( 'NONE',  ( 1.497042530366522461, 18.62819992234354771, 2.161531897785029965 ) ) ;
#17548 = ORIENTED_EDGE ( 'NONE', *, *, #1453, .F. ) ;
#17549 = TOROIDAL_SURFACE ( 'NONE', #13657, 9.000000000000003553, 0.9999999999999991118 ) ;
#17550 = CARTESIAN_POINT ( 'NONE',  ( -3.607379964056306676, 20.24680007765648071, 2.690724712371306282 ) ) ;
#17551 = CARTESIAN_POINT ( 'NONE',  ( -4.000000000000000888, -22.17415986155084795, -7.386502140033922359 ) ) ;
#17552 = ORIENTED_EDGE ( 'NONE', *, *, #4781, .T. ) ;
#17553 = CARTESIAN_POINT ( 'NONE',  ( 0.000000000000000000, 38.59999999999999432, 2.500000000000000000 ) ) ;
#17554 = CARTESIAN_POINT ( 'NONE',  ( -1.027846397803541700, 34.99680007765648071, 3.346150245485522312 ) ) ;
#17555 = CARTESIAN_POINT ( 'NONE',  ( 1.071796769724485232, -28.73013614155210149, -9.775619414081942793 ) ) ;
#17556 = CARTESIAN_POINT ( 'NONE',  ( -2.121784821874996396, -18.83573003411303048, -9.025965403792225672 ) ) ;
#17557 = CARTESIAN_POINT ( 'NONE',  ( -4.243569643749997233, -22.43105049029164277, -12.02487009106222615 ) ) ;
#17558 = CARTESIAN_POINT ( 'NONE',  ( -1.999999999999996225, -20.15388036368618074, -10.54072086271434117 ) ) ;
#17559 = VERTEX_POINT ( 'NONE', #12205 ) ;
#17560 = CARTESIAN_POINT ( 'NONE',  ( 5.954418220269343642, -10.00000000000000178, 20.87519200589467872 ) ) ;
#17561 = CARTESIAN_POINT ( 'NONE',  ( 1.999999999999994449, -24.99027666555753413, -5.368856879811245264 ) ) ;
#17562 = CARTESIAN_POINT ( 'NONE',  ( 1.533898589781675205E-14, -28.22544404955499786, -9.054844408877768203 ) ) ;
#17563 = ORIENTED_EDGE ( 'NONE', *, *, #13749, .F. ) ;
#17564 = CARTESIAN_POINT ( 'NONE',  ( -1.135272562821019626, 29.00319992234354416, 3.311245368580577164 ) ) ;
#17565 = CARTESIAN_POINT ( 'NONE',  ( 9.530870139287183087E-15, 10.00000000000000000, 7.000000000000003553 ) ) ;
#17566 = CARTESIAN_POINT ( 'NONE',  ( 2.121784821874994176, -24.98561633879609545, -4.994442936591867443 ) ) ;
#17567 = CARTESIAN_POINT ( 'NONE',  ( 0.05938372350926800214, 19.87180007765648426, 2.628655560595669183 ) ) ;
#17568 = AXIS2_PLACEMENT_3D ( 'NONE', #6851, #12505, #2789 ) ;
#17569 = ADVANCED_FACE ( 'NONE', ( #15011 ), #13347, .T. ) ;
#17570 = CARTESIAN_POINT ( 'NONE',  ( -3.607379964056363075, 19.75319992234354416, -2.690724712371229899 ) ) ;
#17571=STYLED_ITEM('',(#18396),#1553);
#17572 = CARTESIAN_POINT ( 'NONE',  ( 2.121784821875004390, -24.07319986854348670, -16.50584750820610580 ) ) ;
#17573 = CARTESIAN_POINT ( 'NONE',  ( -5.279047395330986450E-15, -29.76477468405075300, -10.17438775457732625 ) ) ;
#17574 = ADVANCED_FACE ( 'NONE', ( #6556 ), #10975, .T. ) ;
#17575 = CARTESIAN_POINT ( 'NONE',  ( -4.243569643750000786, -23.38404765733129764, -9.114400983959404456 ) ) ;
#17576 = CARTESIAN_POINT ( 'NONE',  ( 4.243569643750003451, -19.16166480309071574, -7.355703438614951573 ) ) ;
#17577 = EDGE_CURVE ( 'NONE', #10853, #244, #4703, .T. ) ;
#17578 = CARTESIAN_POINT ( 'NONE',  ( -6.618784548698717352, -14.16206772970377159, -2.127281972413720634 ) ) ;
#17579 = FACE_OUTER_BOUND ( 'NONE', #1867, .T. ) ;
#17580 = TOROIDAL_SURFACE ( 'NONE', #5699, 9.000000000000001776, 0.9999999999999991118 ) ;
#17581 = DIRECTION ( 'NONE',  ( 0.000000000000000000, 1.000000000000000000, -1.478898702612462246E-15 ) ) ;
#17582 = TOROIDAL_SURFACE ( 'NONE', #5984, 9.000000000000001776, 0.9999999999999991118 ) ;
#17583 = PLANE ( 'NONE',  #2629 ) ;
#17584 = VERTEX_POINT ( 'NONE', #2762 ) ;
#17585 = VERTEX_POINT ( 'NONE', #16678 ) ;
#17586 =( LENGTH_UNIT ( ) NAMED_UNIT ( * ) SI_UNIT ( .MILLI., .METRE. ) );
#17587 = CARTESIAN_POINT ( 'NONE',  ( 1.071796769724485232, -24.08416700710866110, -3.140487855341086654 ) ) ;
#17588 = VECTOR ( 'NONE', #10798, 1000.000000000000000 ) ;
#17589 = FACE_OUTER_BOUND ( 'NONE', #3499, .T. ) ;
#17590 = VERTEX_POINT ( 'NONE', #5712 ) ;
#17591 = CARTESIAN_POINT ( 'NONE',  ( -1.593127413382952939, 31.62819992234354416, 2.091722143975172532 ) ) ;
#17592 = SURFACE_STYLE_USAGE ( .BOTH. , #10598 ) ;
#17593 = CARTESIAN_POINT ( 'NONE',  ( 2.121784821875004390, -23.00849860856686036, -14.98529652599465933 ) ) ;
#17594 = CARTESIAN_POINT ( 'NONE',  ( -2.211161402132902243, 25.87180007765647360, -2.942372952327172886 ) ) ;
#17595 = DIRECTION ( 'NONE',  ( -0.000000000000000000, 1.000000000000000000, 1.224646799147353207E-16 ) ) ;
#17596 = CARTESIAN_POINT ( 'NONE',  ( 0.6435590302261994244, -15.45066141473231980, -10.82404826198633430 ) ) ;
#17597 = CIRCLE ( 'NONE', #17877, 8.000000000000003553 ) ;
#17598 = VECTOR ( 'NONE', #6493, 1000.000000000000000 ) ;
#17599 = CARTESIAN_POINT ( 'NONE',  ( -4.243569643749997233, -23.20537867936554832, -13.13072535085237114 ) ) ;
#17600 =( LENGTH_UNIT ( ) NAMED_UNIT ( * ) SI_UNIT ( .MILLI., .METRE. ) );
#17601 = CARTESIAN_POINT ( 'NONE',  ( 4.243569643749997233, -26.54172925159527097, -9.352547547092401103 ) ) ;
#17602 = LINE ( 'NONE', #3838, #4035 ) ;
#17603 = CARTESIAN_POINT ( 'NONE',  ( -1.734723475976807094E-15, 38.59999999999999432, -11.50000000000000178 ) ) ;
#17604 = CARTESIAN_POINT ( 'NONE',  ( 1.300000000000000044, 0.000000000000000000, 0.000000000000000000 ) ) ;
#17605 = CARTESIAN_POINT ( 'NONE',  ( -5.330712181944245322E-15, -27.04303497500847797, -5.796996205112000311 ) ) ;
#17606 = ORIENTED_EDGE ( 'NONE', *, *, #16594, .F. ) ;
#17607 = CARTESIAN_POINT ( 'NONE',  ( -8.500000000000005329, 10.00000000000000000, -22.50000000000000000 ) ) ;
#17608 = CIRCLE ( 'NONE', #9578, 4.000000000000000888 ) ;
#17609 = DIRECTION ( 'NONE',  ( -1.000000000000000000, 0.000000000000000000, 1.053778523157998394E-14 ) ) ;
#17610 = CARTESIAN_POINT ( 'NONE',  ( 1.989345975306426206, 28.99680007765648071, -1.515154207786343799 ) ) ;
#17611 = VERTEX_POINT ( 'NONE', #12569 ) ;
#17612 = CARTESIAN_POINT ( 'NONE',  ( 1.027846397803542144, 28.74680007765647716, -3.346150245485522312 ) ) ;
#17613 = EDGE_CURVE ( 'NONE', #18256, #8069, #14186, .T. ) ;
#17614 = CARTESIAN_POINT ( 'NONE',  ( 1.071796769724494780, -27.24600711319871493, -7.656063500490938978 ) ) ;
#17615 = CONTEXT_DEPENDENT_SHAPE_REPRESENTATION ( #13884, #7965 ) ;
#17616 = CARTESIAN_POINT ( 'NONE',  ( 4.000000000000000888, -20.30286673866052283, -4.714018596547838946 ) ) ;
#17617 = CARTESIAN_POINT ( 'NONE',  ( -1.135272562821019626, 21.50319992234354416, 3.311245368580577164 ) ) ;
#17618 = ORIENTED_EDGE ( 'NONE', *, *, #7508, .F. ) ;
#17619 = CARTESIAN_POINT ( 'NONE',  ( -5.330712181944246111E-15, -27.07529864955322552, -5.843073507603255834 ) ) ;
#17620 = CARTESIAN_POINT ( 'NONE',  ( -2.211161402132902243, 15.87180007765647716, -2.942372952327172886 ) ) ;
#17621 = EDGE_LOOP ( 'NONE', ( #824, #16759, #6755, #12528, #8678 ) ) ;
#17622 = VECTOR ( 'NONE', #17498, 1000.000000000000000 ) ;
#17623 = PRODUCT ( 'seal', 'seal', '', ( #13580 ) ) ;
#17624 = DIRECTION ( 'NONE',  ( 1.000000000000000000, 0.000000000000000000, 0.000000000000000000 ) ) ;
#17625 = CARTESIAN_POINT ( 'NONE',  ( 4.243569643750003451, -23.03330574846024703, -12.88497973756566672 ) ) ;
#17626 = CARTESIAN_POINT ( 'NONE',  ( -1.999999999999996225, -22.54139228070233614, -13.95044124807404451 ) ) ;
#17627 = CARTESIAN_POINT ( 'NONE',  ( 7.484523392482447690, -12.68578631963116621, 7.186755514441455439 ) ) ;
#17628 = FACE_OUTER_BOUND ( 'NONE', #11037, .T. ) ;
#17629 = CARTESIAN_POINT ( 'NONE',  ( -5.330712181944245322E-15, -24.23609528961556947, -1.788270888372730960 ) ) ;
#17630 = EDGE_CURVE ( 'NONE', #4921, #6179, #28, .T. ) ;
#17631 = EDGE_LOOP ( 'NONE', ( #796, #7765, #10939, #5625 ) ) ;
#17632 = DIRECTION ( 'NONE',  ( -0.000000000000000000, -0.000000000000000000, -1.000000000000000000 ) ) ;
#17633 = CARTESIAN_POINT ( 'NONE',  ( -3.999999999999997335, -20.88466450731445079, -9.571229827256534151 ) ) ;
#17634 = EDGE_CURVE ( 'NONE', #5980, #7871, #14243, .T. ) ;
#17635 = ORIENTED_EDGE ( 'NONE', *, *, #3276, .T. ) ;
#17636 = ORIENTED_EDGE ( 'NONE', *, *, #3454, .T. ) ;
#17637 =( BOUNDED_CURVE ( )  B_SPLINE_CURVE ( 2, ( #15554, #17232, #10054, #3029, #7276, #16198, #6072, #3489, #16015 ),
 .UNSPECIFIED., .F., .T. ) 
 B_SPLINE_CURVE_WITH_KNOTS ( ( 3, 2, 2, 2, 3 ),
 ( 0.4224137931034482873, 0.4252873563218390607, 0.4310344827586206629, 0.4367816091954023205, 0.4396551724137931494 ),
 .UNSPECIFIED. ) 
 CURVE ( )  GEOMETRIC_REPRESENTATION_ITEM ( )  RATIONAL_B_SPLINE_CURVE ( ( 0.9330127018922194093, 0.9330127018922200755, 1.000000000000000000, 0.8660254037844387076, 1.000000000000000000, 0.8660254037844387076, 1.000000000000000000, 0.9330127018922187432, 0.9330127018922194093 ) ) 
 REPRESENTATION_ITEM ( '' )  );
#17638 = CARTESIAN_POINT ( 'NONE',  ( -1.734723475976807094E-15, 38.59999999999999432, -12.50000000000000000 ) ) ;
#17639 = DIRECTION ( 'NONE',  ( -4.915049848600951133E-16, 0.000000000000000000, -1.000000000000000000 ) ) ;
#17640 = EDGE_CURVE ( 'NONE', #9378, #6645, #9198, .T. ) ;
#17641 = CARTESIAN_POINT ( 'NONE',  ( -4.499999999999999112, 27.00319992234355126, -0.05647727720528529505 ) ) ;
#17642 = CARTESIAN_POINT ( 'NONE',  ( -0.05938372350920064630, 38.87819992234354061, 3.680117784833935701 ) ) ;
#17643 = CARTESIAN_POINT ( 'NONE',  ( 2.055738996568281518, 18.00319992234354416, -1.423772053676066518 ) ) ;
#17644 = EDGE_LOOP ( 'NONE', ( #5187, #4274, #2610, #6902 ) ) ;
#17645 = CARTESIAN_POINT ( 'NONE',  ( 3.607379964056363075, 38.50319992234354771, 2.690724712371229010 ) ) ;
#17646 = CARTESIAN_POINT ( 'NONE',  ( 4.000000000000003553, -20.13184543389876779, -8.496092768120460548 ) ) ;
#17647 = ORIENTED_EDGE ( 'NONE', *, *, #6077, .F. ) ;
#17648 = DIRECTION ( 'NONE',  ( -0.000000000000000000, -1.000000000000000000, -0.000000000000000000 ) ) ;
#17649 = CARTESIAN_POINT ( 'NONE',  ( -1.135272562821090014, 35.99680007765648071, -3.311245368580554072 ) ) ;
#17650 = CARTESIAN_POINT ( 'NONE',  ( -11.99999999999999822, 13.00000000000000178, 15.00000000000000000 ) ) ;
#17651 = CARTESIAN_POINT ( 'NONE',  ( 2.121784821874994176, -23.17885056429031465, -2.414113997081532847 ) ) ;
#17652 = CARTESIAN_POINT ( 'NONE',  ( -4.243569643750005227, -26.40191999523469946, -9.152879236296964649 ) ) ;
#17653 = CARTESIAN_POINT ( 'NONE',  ( -2.000000000000005773, -25.74309573756332270, -6.443993936933789968 ) ) ;
#17654 = VERTEX_POINT ( 'NONE', #16863 ) ;
#17655 = CARTESIAN_POINT ( 'NONE',  ( -6.097036691290805166, -11.55344374157283660, 15.47841750116366377 ) ) ;
#17656 = DIRECTION ( 'NONE',  ( 0.000000000000000000, 0.000000000000000000, 1.000000000000000000 ) ) ;
#17657 = CARTESIAN_POINT ( 'NONE',  ( -9.000000000000001776, 20.99999999999999289, 2.499999999999998224 ) ) ;
#17658 = CARTESIAN_POINT ( 'NONE',  ( 2.121784821874994176, -29.66384914778427628, -11.67565179782398310 ) ) ;
#17659 = ORIENTED_EDGE ( 'NONE', *, *, #15525, .F. ) ;
#17660 = CARTESIAN_POINT ( 'NONE',  ( 3.500000000000000444, 25.75319992234354771, 0.05647727720529520379 ) ) ;
#17661 = CARTESIAN_POINT ( 'NONE',  ( 3.481649420246395010, 15.87819992234354416, 1.193696214020467439 ) ) ;
#17662 = CARTESIAN_POINT ( 'NONE',  ( 4.243569643750000786, -21.67407290645975948, -6.672303951922835097 ) ) ;
#17663 = CARTESIAN_POINT ( 'NONE',  ( -1.989345975306426206, 25.24680007765648071, 1.515154207786343799 ) ) ;
#17664 = CARTESIAN_POINT ( 'NONE',  ( -3.518350579753605434, 39.37819992234354771, 1.080741659609877781 ) ) ;
#17665 = CARTESIAN_POINT ( 'NONE',  ( -2.121784821874996396, -23.25585344674324162, -15.33855584509429271 ) ) ;
#17666 = CARTESIAN_POINT ( 'NONE',  ( 3.999999999999996447, -28.08811523457247006, -11.80618781089809488 ) ) ;
#17667 = CARTESIAN_POINT ( 'NONE',  ( 2.121784821875004390, -17.87857435595223876, -7.659005429884962801 ) ) ;
#17668 = CARTESIAN_POINT ( 'NONE',  ( 4.518350579753633411, 39.37180007765647360, 1.405661355842698468 ) ) ;
#17669 = CARTESIAN_POINT ( 'NONE',  ( -1.734723475976807094E-15, 36.39999999999999147, -2.500000000000000000 ) ) ;
#17670 = CARTESIAN_POINT ( 'NONE',  ( 4.000000000000003553, -18.32507965939299055, -5.915763828610125508 ) ) ;
#17671 = CARTESIAN_POINT ( 'NONE',  ( 3.250762944584260072, -21.87258937905581746, -2.200190645090608133 ) ) ;
#17672 = VERTEX_POINT ( 'NONE', #3957 ) ;
#17673 = VERTEX_POINT ( 'NONE', #5348 ) ;
#17674 = CARTESIAN_POINT ( 'NONE',  ( 3.250762944584260516, -21.87258937905581746, -2.200190645090608133 ) ) ;
#17675 = EDGE_CURVE ( 'NONE', #6645, #9378, #1222, .T. ) ;
#17676 = CYLINDRICAL_SURFACE ( 'NONE', #10106, 0.9999999999999991118 ) ;
#17677 = CARTESIAN_POINT ( 'NONE',  ( 6.428571428571431490, -11.73421655796352425, 14.25837509840157935 ) ) ;
#17678 = ORIENTED_EDGE ( 'NONE', *, *, #5649, .T. ) ;
#17679 = CARTESIAN_POINT ( 'NONE',  ( 2.481649420246391902, 30.87819992234354416, 0.8687765177875720335 ) ) ;
#17680 = CARTESIAN_POINT ( 'NONE',  ( -4.243569643749997233, -23.68933379753673663, -13.82188488822120931 ) ) ;
#17681 = CARTESIAN_POINT ( 'NONE',  ( 1.135272562821090458, 22.24680007765648071, 3.311245368580554072 ) ) ;
#17682 = EDGE_CURVE ( 'NONE', #14789, #6640, #11553, .T. ) ;
#17683 = DIRECTION ( 'NONE',  ( 0.000000000000000000, 0.000000000000000000, -1.000000000000000000 ) ) ;
#17684 = VECTOR ( 'NONE', #11803, 1000.000000000000000 ) ;
#17685 = CARTESIAN_POINT ( 'NONE',  ( 1.281796014811036999, -15.42359483004404730, -10.64137488400890597 ) ) ;
#17686 = CARTESIAN_POINT ( 'NONE',  ( 4.243569643750003451, -24.06574333389212228, -14.35945341728585767 ) ) ;
#17687 = LINE ( 'NONE', #6623, #1678 ) ;
#17688 = CARTESIAN_POINT ( 'NONE',  ( 4.005420803925811235, -27.01550616763517709, -14.30066121701663029 ) ) ;
#17689 = DIRECTION ( 'NONE',  ( -0.000000000000000000, 1.000000000000000000, -0.000000000000000000 ) ) ;
#17690 = AXIS2_PLACEMENT_3D ( 'NONE', #3298, #1920, #7547 ) ;
#17691 = CARTESIAN_POINT ( 'NONE',  ( 4.243569643749996345, -24.99307287344746342, -7.140837027512114688 ) ) ;
#17692 = VERTEX_POINT ( 'NONE', #6996 ) ;
#17693 = LINE ( 'NONE', #17607, #17228 ) ;
#17694 = CARTESIAN_POINT ( 'NONE',  ( -3.500000000000000000, 15.00000000000000355, 3.564992268403899267E-14 ) ) ;
#17695 = CARTESIAN_POINT ( 'NONE',  ( 1.593127413382998903, 32.12180007765648071, 2.091722143975139669 ) ) ;
#17696 = EDGE_CURVE ( 'NONE', #3919, #17357, #14545, .T. ) ;
#17697 = ORIENTED_EDGE ( 'NONE', *, *, #16123, .F. ) ;
#17698 = CARTESIAN_POINT ( 'NONE',  ( -1.027846397803541700, 29.99680007765648071, 3.346150245485522312 ) ) ;
#17699 = CARTESIAN_POINT ( 'NONE',  ( -4.000000000000000888, -26.62654694943075029, -13.74516988483401114 ) ) ;
#17700 = PRODUCT_CONTEXT ( 'NONE', #9141, 'mechanical' ) ;
#17701 = CARTESIAN_POINT ( 'NONE',  ( 9.530870139287183087E-15, 13.00000000000000178, 7.000000000000003553 ) ) ;
#17702 =( REPRESENTATION_RELATIONSHIP ('NONE','NONE', #15868, #4006 ) REPRESENTATION_RELATIONSHIP_WITH_TRANSFORMATION ( #12369 )SHAPE_REPRESENTATION_RELATIONSHIP( ) );
#17703 = ORIENTED_EDGE ( 'NONE', *, *, #4223, .T. ) ;
#17704 = CARTESIAN_POINT ( 'NONE',  ( -5.330712181944246111E-15, -26.30097046047931997, -4.737218247813112626 ) ) ;
#17705 = CARTESIAN_POINT ( 'NONE',  ( 2.798362969681366330, 18.99680007765648071, -2.102939460078824929 ) ) ;
#17706 = AXIS2_PLACEMENT_3D ( 'NONE', #4932, #13546, #14877 ) ;
#17707 = ORIENTED_EDGE ( 'NONE', *, *, #8416, .F. ) ;
#17708 = SURFACE_SIDE_STYLE ('',( #635 ) ) ;
#17709 = DIRECTION ( 'NONE',  ( -1.000000000000000000, 0.000000000000000000, 4.336808689942021680E-16 ) ) ;
#17710 = CARTESIAN_POINT ( 'NONE',  ( -3.446515024960077778, -28.75821711830315408, -13.15225657165725082 ) ) ;
#17711 = CYLINDRICAL_SURFACE ( 'NONE', #14087, 2.149999999999995470 ) ;
#17712 = DIRECTION ( 'NONE',  ( -1.000000000000000000, 0.000000000000000000, 4.336808689942021680E-16 ) ) ;
#17713 = CARTESIAN_POINT ( 'NONE',  ( -1.071796769724477238, -24.94607594741468048, -4.371421390432334242 ) ) ;
#17714 = CARTESIAN_POINT ( 'NONE',  ( 2.121784821875004390, -16.84613677052036351, -6.184531750164772745 ) ) ;
#17715 = ORIENTED_EDGE ( 'NONE', *, *, #10156, .T. ) ;
#17716 = CARTESIAN_POINT ( 'NONE',  ( 0.000000000000000000, 5.977523610840987267, 32.81826849749789687 ) ) ;
#17717 = CARTESIAN_POINT ( 'NONE',  ( -3.999999999999997335, -21.40088330003038664, -10.30846666711663140 ) ) ;
#17718 = CIRCLE ( 'NONE', #10008, 6.000000000000000888 ) ;
#17719 = ORIENTED_EDGE ( 'NONE', *, *, #9098, .T. ) ;
#17720 = AXIS2_PLACEMENT_3D ( 'NONE', #1846, #732, #13139 ) ;
#17721 = EDGE_LOOP ( 'NONE', ( #15454, #13978, #11253, #5551 ) ) ;
#17722 = FACE_OUTER_BOUND ( 'NONE', #13905, .T. ) ;
#17723 = CARTESIAN_POINT ( 'NONE',  ( 1.444289557195957086, 27.75319992234354416, -4.262301884875733471 ) ) ;
#17724 = CARTESIAN_POINT ( 'NONE',  ( -3.518350579753606322, 39.37819992234354771, 1.080741659609877781 ) ) ;
#17725 = CARTESIAN_POINT ( 'NONE',  ( -1.497042530366522461, 22.37819992234354416, -2.161531897785030409 ) ) ;
#17726 = ORIENTED_EDGE ( 'NONE', *, *, #14411, .F. ) ;
#17727 = CARTESIAN_POINT ( 'NONE',  ( 1.444289557196047680, 17.24680007765648071, 4.262301884875704161 ) ) ;
#17728 = CARTESIAN_POINT ( 'NONE',  ( 4.000000000000003553, -20.38995483025674105, -8.864711188050506507 ) ) ;
#17729 = VERTEX_POINT ( 'NONE', #18349 ) ;
#17730 = ADVANCED_FACE ( 'NONE', ( #15375 ), #4231, .T. ) ;
#17731 = COLOUR_RGB ( '',0.8941176470588234615, 0.8941176470588234615, 0.8941176470588234615 ) ;
#17732 = FACE_OUTER_BOUND ( 'NONE', #2581, .T. ) ;
#17733 = ADVANCED_FACE ( 'NONE', ( #9874 ), #1189, .F. ) ;
#17734 = CIRCLE ( 'NONE', #14151, 0.4000000000000006883 ) ;
#17735 = CARTESIAN_POINT ( 'NONE',  ( -2.864755990943265829, 38.24680007765647360, -2.011557305968488141 ) ) ;
#17736 = CARTESIAN_POINT ( 'NONE',  ( 9.000000000000005329, 31.99999999999999289, 2.499999999999997335 ) ) ;
#17737 = ADVANCED_FACE ( 'NONE', ( #1094 ), #11001, .F. ) ;
#17738 = CARTESIAN_POINT ( 'NONE',  ( -4.243569643749998122, -18.78525526673533719, -6.818134909550301437 ) ) ;
#17739 =( BOUNDED_CURVE ( )  B_SPLINE_CURVE ( 2, ( #17340, #12013, #3318, #727, #6184, #15929, #11644, #13038, #1839 ),
 .UNSPECIFIED., .F., .F. ) 
 B_SPLINE_CURVE_WITH_KNOTS ( ( 3, 2, 2, 2, 3 ),
 ( 0.7500000000000000000, 0.7528735632183908288, 0.7586206896551723755, 0.7643678160919540332, 0.7672413793103448620 ),
 .UNSPECIFIED. ) 
 CURVE ( )  GEOMETRIC_REPRESENTATION_ITEM ( )  RATIONAL_B_SPLINE_CURVE ( ( 0.9330127018922194093, 0.9330127018922194093, 1.000000000000000000, 0.8660254037844387076, 1.000000000000000000, 0.8660254037844387076, 1.000000000000000000, 0.9330127018922180770, 0.9330127018922194093 ) ) 
 REPRESENTATION_ITEM ( '' )  );
#17740 = CARTESIAN_POINT ( 'NONE',  ( 4.243569643750000786, -24.80364933730013277, -11.14180229357466345 ) ) ;
#17741 = EDGE_CURVE ( 'NONE', #3578, #1058, #5056, .T. ) ;
#17742 = DIRECTION ( 'NONE',  ( 0.000000000000000000, -1.000000000000000000, 0.000000000000000000 ) ) ;
#17743 = ORIENTED_EDGE ( 'NONE', *, *, #4226, .F. ) ;
#17744 = CARTESIAN_POINT ( 'NONE',  ( 4.386042834387938960, -10.00000000000000178, 22.42214358049745826 ) ) ;
#17745 = FILL_AREA_STYLE ('',( #12050 ) ) ;
#17746 = PRESENTATION_STYLE_ASSIGNMENT (( #15127 ) ) ;
#17747 = CARTESIAN_POINT ( 'NONE',  ( -3.706921591972381904E-14, -19.54282517599473579, -10.60235393626997080 ) ) ;
#17748 = ORIENTED_EDGE ( 'NONE', *, *, #4953, .T. ) ;
#17749 = CARTESIAN_POINT ( 'NONE',  ( -2.798362969681409851, 29.75319992234354416, -2.102939460078765421 ) ) ;
#17750 = FACE_OUTER_BOUND ( 'NONE', #6258, .T. ) ;
#17751 = VECTOR ( 'NONE', #7891, 1000.000000000000000 ) ;
#17752 = CARTESIAN_POINT ( 'NONE',  ( 4.730628863548789710E-15, -16.04700144155306774, -7.178993278803624811 ) ) ;
#17753 = CARTESIAN_POINT ( 'NONE',  ( 0.8262555684461332373, 19.74680007765648071, 2.360188852285403982 ) ) ;
#17754 = EDGE_CURVE ( 'NONE', #3449, #4719, #4765, .T. ) ;
#17755 = CARTESIAN_POINT ( 'NONE',  ( 4.499999999999999112, 20.75319992234354416, 0.05647727720528474687 ) ) ;
#17756 = CARTESIAN_POINT ( 'NONE',  ( 1.999999999999994449, -28.53928086477465698, -10.43736015284263807 ) ) ;
#17757 = ORIENTED_EDGE ( 'NONE', *, *, #10488, .T. ) ;
#17758 = CARTESIAN_POINT ( 'NONE',  ( -4.243569643750005227, -22.78838844622314497, -3.992221357276296345 ) ) ;
#17759 = CARTESIAN_POINT ( 'NONE',  ( 3.481649420246369697, 16.62180007765648071, -1.193696214020541824 ) ) ;
#17760 = CIRCLE ( 'NONE', #9723, 2.149999999999995470 ) ;
#17761 = AXIS2_PLACEMENT_3D ( 'NONE', #14376, #7313, #290 ) ;
#17762 = B_SPLINE_CURVE_WITH_KNOTS ( 'NONE', 1,
 ( #16490, #10997 ),
 .UNSPECIFIED., .F., .F.,
 ( 2, 2 ),
 ( 0.6192647773654433863, 1.000000000000000000 ),
 .UNSPECIFIED. ) ;
#17763 = DIRECTION ( 'NONE',  ( 3.469446951953612217E-16, -0.000000000000000000, 1.000000000000000000 ) ) ;
#17764 = DIRECTION ( 'NONE',  ( 0.000000000000000000, 0.000000000000000000, 1.000000000000000000 ) ) ;
#17765 = DIRECTION ( 'NONE',  ( 0.000000000000000000, 0.000000000000000000, -1.000000000000000000 ) ) ;
#17766 = VERTEX_POINT ( 'NONE', #338 ) ;
#17767 = VERTEX_POINT ( 'NONE', #4775 ) ;
#17768 = CARTESIAN_POINT ( 'NONE',  ( 4.730628863548789710E-15, -15.78889204519509981, -6.810374858873577075 ) ) ;
#17769 = DIRECTION ( 'NONE',  ( 1.000000000000000000, 0.000000000000000000, 0.000000000000000000 ) ) ;
#17770 = CARTESIAN_POINT ( 'NONE',  ( 4.000000000000000888, -24.10998033423561893, -10.15114028950927683 ) ) ;
#17771 = EDGE_LOOP ( 'NONE', ( #11248, #17636, #1468, #16414 ) ) ;
#17772 = CARTESIAN_POINT ( 'NONE',  ( -1.593127413382952939, 29.12819992234354416, 2.091722143975172532 ) ) ;
#17773 = CARTESIAN_POINT ( 'NONE',  ( 0.000000000000000000, 0.000000000000000000, 0.000000000000000000 ) ) ;
#17774 = CARTESIAN_POINT ( 'NONE',  ( 4.243569643750000786, -25.80382324818726048, -12.57019867080359710 ) ) ;
#17775 = CARTESIAN_POINT ( 'NONE',  ( 0.05938372350927906274, 19.87180007765648426, 3.680117784833935701 ) ) ;
#17776 = AXIS2_PLACEMENT_3D ( 'NONE', #3939, #10802, #18153 ) ;
#17777 = AXIS2_PLACEMENT_3D ( 'NONE', #7845, #13498, #812 ) ;
#17778 = CARTESIAN_POINT ( 'NONE',  ( 0.000000000000000000, 46.00000000000000000, 2.500000000000000000 ) ) ;
#17779 = CIRCLE ( 'NONE', #12702, 0.9999999999999991118 ) ;
#17780 = CARTESIAN_POINT ( 'NONE',  ( 1.794514420735380256, -10.00000000000000178, -12.33839425357223618 ) ) ;
#17781 = CARTESIAN_POINT ( 'NONE',  ( 4.243569643750000786, -25.06175873365810247, -11.51042071350471119 ) ) ;
#17782 = CARTESIAN_POINT ( 'NONE',  ( 10.00000000000000355, 31.99999999999999289, 2.499999999999996891 ) ) ;
#17783 = AXIS2_PLACEMENT_3D ( 'NONE', #5371, #6752, #9805 ) ;
#17784 = FACE_OUTER_BOUND ( 'NONE', #12668, .T. ) ;
#17785 = LINE ( 'NONE', #10700, #17436 ) ;
#17786 = CARTESIAN_POINT ( 'NONE',  ( 4.243569643750003451, -21.19427629940971869, -10.25857349556407527 ) ) ;
#17787 = CARTESIAN_POINT ( 'NONE',  ( -10.00000000000000000, 23.19999999999999574, 2.499999999999996003 ) ) ;
#17788 = CARTESIAN_POINT ( 'NONE',  ( -8.500000000000005329, 0.000000000000000000, 18.49999999999999645 ) ) ;
#17789 = CARTESIAN_POINT ( 'NONE',  ( -2.481649420246374138, 32.87180007765648071, 0.8687765177876256573 ) ) ;
#17790 = ORIENTED_EDGE ( 'NONE', *, *, #10800, .F. ) ;
#17791 = SHAPE_REPRESENTATION ( 'Brass Valve Body', ( #16940 ), #12175 ) ;
#17792 = CARTESIAN_POINT ( 'NONE',  ( 2.864755990943265829, 29.49680007765647716, 2.011557305968487697 ) ) ;
#17793 = DIRECTION ( 'NONE',  ( 0.000000000000000000, 0.000000000000000000, 1.000000000000000000 ) ) ;
#17794 = PRODUCT_CONTEXT ( 'NONE', #13285, 'mechanical' ) ;
#17795 = DIRECTION ( 'NONE',  ( 3.469446951953614189E-16, -0.000000000000000000, 1.000000000000000000 ) ) ;
#17796 = ORIENTED_EDGE ( 'NONE', *, *, #5247, .T. ) ;
#17797 = CARTESIAN_POINT ( 'NONE',  ( 2.121784821875004390, -20.20155892317395541, -10.97657120925539154 ) ) ;
#17798 = AXIS2_PLACEMENT_3D ( 'NONE', #2377, #12179, #3572 ) ;
#17799 = CARTESIAN_POINT ( 'NONE',  ( -2.211161402132902243, 23.37180007765647716, -2.942372952327172886 ) ) ;
#17800 = EDGE_LOOP ( 'NONE', ( #13800, #17757, #15014, #562 ) ) ;
#17801 = CARTESIAN_POINT ( 'NONE',  ( -10.00000000000000000, 18.79999999999999361, 2.499999999999998224 ) ) ;
#17802 = ADVANCED_FACE ( 'NONE', ( #5977 ), #14241, .T. ) ;
#17803 = FACE_OUTER_BOUND ( 'NONE', #8956, .T. ) ;
#17804 = DIRECTION ( 'NONE',  ( 0.000000000000000000, 1.000000000000000000, 0.000000000000000000 ) ) ;
#17805 = CARTESIAN_POINT ( 'NONE',  ( 9.604546805300321566, -9.971739665363084981, 12.06860958386529781 ) ) ;
#17806 = CARTESIAN_POINT ( 'NONE',  ( 4.898587196589412829E-16, 10.00000000000000000, -4.000000000000000000 ) ) ;
#17807 = CARTESIAN_POINT ( 'NONE',  ( 3.250762944584260516, -21.90485305360056145, -2.246267947581864100 ) ) ;
#17808 = VERTEX_POINT ( 'NONE', #10236 ) ;
#17809 = CARTESIAN_POINT ( 'NONE',  ( -8.000000000000003553, 34.19999999999999574, -2.500000000000001776 ) ) ;
#17810 = CARTESIAN_POINT ( 'NONE',  ( -2.000000000000005773, -25.29140429464182560, -5.798911703062972656 ) ) ;
#17811 = CIRCLE ( 'NONE', #15133, 0.9999999999999991118 ) ;
#17812 = CARTESIAN_POINT ( 'NONE',  ( 0.05938372350927906274, 34.87180007765645939, 3.680117784833935701 ) ) ;
#17813 = ORIENTED_EDGE ( 'NONE', *, *, #3276, .F. ) ;
#17814 = EDGE_LOOP ( 'NONE', ( #12962, #12938, #13047, #16227, #14203, #4443, #125, #3240, #4216 ) ) ;
#17815 = FACE_OUTER_BOUND ( 'NONE', #12977, .T. ) ;
#17816 = CARTESIAN_POINT ( 'NONE',  ( -1.336863392178569088, 32.50319992234354771, -4.297206761780648421 ) ) ;
#17817 = CARTESIAN_POINT ( 'NONE',  ( -2.798362969681409851, 37.25319992234354061, -2.102939460078765421 ) ) ;
#17818 = CARTESIAN_POINT ( 'NONE',  ( -0.05938372350921170689, 26.37819992234355126, 2.628655560595669183 ) ) ;
#17819 = ORIENTED_EDGE ( 'NONE', *, *, #12711, .T. ) ;
#17820 = CARTESIAN_POINT ( 'NONE',  ( -3.673772985318219053, 18.24680007765647716, -2.599342558260952174 ) ) ;
#17821 = CARTESIAN_POINT ( 'NONE',  ( 2.000000000000004441, -17.87391402919079653, -7.284591486665584981 ) ) ;
#17822 = ORIENTED_EDGE ( 'NONE', *, *, #17386, .F. ) ;
#17823 = DIRECTION ( 'NONE',  ( 0.000000000000000000, 0.8191520442889952403, -0.5735764363510413855 ) ) ;
#17824 = CARTESIAN_POINT ( 'NONE',  ( -1.027846397803541700, 37.49680007765647360, 3.346150245485522312 ) ) ;
#17825 = CARTESIAN_POINT ( 'NONE',  ( 1.999999999999994449, -26.73251509026887618, -7.857031213332303921 ) ) ;
#17826 = CARTESIAN_POINT ( 'NONE',  ( -2.121784821875005722, -23.47997819337460257, -2.844168820333258907 ) ) ;
#17827 = CARTESIAN_POINT ( 'NONE',  ( -4.243569643749997233, -21.91483169757570693, -11.28763325120213068 ) ) ;
#17828 = CARTESIAN_POINT ( 'NONE',  ( -0.7766474010173821663, -30.24966125638259840, -12.04527715262853604 ) ) ;
#17829 = ORIENTED_EDGE ( 'NONE', *, *, #7260, .T. ) ;
#17830 = CARTESIAN_POINT ( 'NONE',  ( -2.000000000000005773, -22.64578298126770051, -2.020572897773216692 ) ) ;
#17831 = EDGE_CURVE ( 'NONE', #6378, #3053, #6607, .T. ) ;
#17832 = CARTESIAN_POINT ( 'NONE',  ( 9.000000000000003553, -4.000000000000000000, 30.00000000000000000 ) ) ;
#17833 = CARTESIAN_POINT ( 'NONE',  ( -4.243569643749997233, -24.49592566115538972, -14.97381745050260804 ) ) ;
#17834 = ORIENTED_EDGE ( 'NONE', *, *, #12935, .F. ) ;
#17835 = CARTESIAN_POINT ( 'NONE',  ( -2.115076519116425580, 37.37819992234352640, -3.012182706137062738 ) ) ;
#17836 = CARTESIAN_POINT ( 'NONE',  ( -1.041744090737314776, 15.00160208984915755, -3.341881251993961133 ) ) ;
#17837 = CARTESIAN_POINT ( 'NONE',  ( 2.121784821875004390, -17.07198249233357856, -6.507072867603563182 ) ) ;
#17838 = CARTESIAN_POINT ( 'NONE',  ( 2.055738996568313048, 24.49680007765648426, 1.423772053676023441 ) ) ;
#17839 = ADVANCED_FACE ( 'NONE', ( #4587 ), #3211, .F. ) ;
#17840 = CARTESIAN_POINT ( 'NONE',  ( -2.864755990943222308, 39.25319992234354771, 2.011557305968548093 ) ) ;
#17841 = CARTESIAN_POINT ( 'NONE',  ( 4.000000000000003553, -23.48726758655236324, -13.28813222721107934 ) ) ;
#17842 = EDGE_LOOP ( 'NONE', ( #6668, #11028, #8610, #12161 ) ) ;
#17843 = CARTESIAN_POINT ( 'NONE',  ( 4.243569643750000786, -21.44822718464654088, -6.349762834484042884 ) ) ;
#17844 = CARTESIAN_POINT ( 'NONE',  ( 2.115076519116362963, 16.37180007765647716, -3.012182706137107147 ) ) ;
#17845 = CARTESIAN_POINT ( 'NONE',  ( 0.000000000000000000, 0.000000000000000000, 0.000000000000000000 ) ) ;
#17846 = DIRECTION ( 'NONE',  ( 0.000000000000000000, 0.8191520442889952403, -0.5735764363510413855 ) ) ;
#17847 = DIRECTION ( 'NONE',  ( -0.000000000000000000, -0.5735764363510414965, -0.8191520442889950182 ) ) ;
#17848 = ORIENTED_EDGE ( 'NONE', *, *, #1747, .F. ) ;
#17849 = ORIENTED_EDGE ( 'NONE', *, *, #18191, .F. ) ;
#17850 = DIRECTION ( 'NONE',  ( 3.469446951953612217E-16, -0.000000000000000000, 1.000000000000000000 ) ) ;
#17851 = EDGE_CURVE ( 'NONE', #6628, #2835, #1519, .T. ) ;
#17852 = EDGE_CURVE ( 'NONE', #10853, #1671, #1823, .T. ) ;
#17853 = TOROIDAL_SURFACE ( 'NONE', #16070, 9.000000000000003553, 0.9999999999999991118 ) ;
#17854 = CARTESIAN_POINT ( 'NONE',  ( 2.000000000000004441, -23.87495749521851351, -15.85496975104595840 ) ) ;
#17855 = DIRECTION ( 'NONE',  ( 0.000000000000000000, 0.000000000000000000, -1.000000000000000000 ) ) ;
#17856 = ORIENTED_EDGE ( 'NONE', *, *, #5856, .T. ) ;
#17857 = VECTOR ( 'NONE', #6671, 1000.000000000000114 ) ;
#17858 = CARTESIAN_POINT ( 'NONE',  ( -2.518350579753611207, 34.37819992234354771, 0.7558219633769609480 ) ) ;
#17859 = EDGE_CURVE ( 'NONE', #11611, #13188, #15440, .T. ) ;
#17860 = CARTESIAN_POINT ( 'NONE',  ( -4.243569643749997233, -22.14067741938892908, -11.61017436864092112 ) ) ;
#17861 = CARTESIAN_POINT ( 'NONE',  ( -1.027846397803541700, 22.49680007765648071, 3.346150245485522312 ) ) ;
#17862 = DIRECTION ( 'NONE',  ( 0.000000000000000000, 0.000000000000000000, -1.000000000000000000 ) ) ;
#17863 = CARTESIAN_POINT ( 'NONE',  ( 1.622307724309302010E-14, -9.999999999999998224, -3.075850967158335614 ) ) ;
#17864 = AXIS2_PLACEMENT_3D ( 'NONE', #1271, #11430, #8562 ) ;
#17865 = CARTESIAN_POINT ( 'NONE',  ( 4.243569643749996345, -27.60643051157189731, -10.87309852930384935 ) ) ;
#17866 = CARTESIAN_POINT ( 'NONE',  ( 0.000000000000000000, -3.518949890710769246, 4.119968255444916849E-15 ) ) ;
#17867 = CARTESIAN_POINT ( 'NONE',  ( -4.499999999999999112, 25.49680007765647716, 0.05647727720537927543 ) ) ;
#17868 = LINE ( 'NONE', #2283, #9763 ) ;
#17869 = FACE_OUTER_BOUND ( 'NONE', #9985, .T. ) ;
#17870 = CARTESIAN_POINT ( 'NONE',  ( -4.243569643750005227, -24.04667175346823527, -5.789236154435278614 ) ) ;
#17871 = ORIENTED_EDGE ( 'NONE', *, *, #10652, .F. ) ;
#17872 = LINE ( 'NONE', #5141, #17588 ) ;
#17873 = CARTESIAN_POINT ( 'NONE',  ( -8.500000000000005329, 0.000000000000000000, 22.50000000000000000 ) ) ;
#17874 = CARTESIAN_POINT ( 'NONE',  ( 2.481649420246374138, 31.62180007765648426, -0.8687765177876252132 ) ) ;
#17875 = FACE_OUTER_BOUND ( 'NONE', #12776, .T. ) ;
#17876 = CARTESIAN_POINT ( 'NONE',  ( 3.500000000000000444, 29.24680007765647716, -0.05647727720536935281 ) ) ;
#17877 = AXIS2_PLACEMENT_3D ( 'NONE', #3755, #8108, #13767 ) ;
#17878 = CIRCLE ( 'NONE', #8969, 2.200000000000000622 ) ;
#17879 = CARTESIAN_POINT ( 'NONE',  ( 8.500000000000001776, 15.00000000000000178, -20.49999999999999645 ) ) ;
#17880 = ORIENTED_EDGE ( 'NONE', *, *, #5369, .T. ) ;
#17881 = CARTESIAN_POINT ( 'NONE',  ( 4.243569643749997233, -22.96046137712846047, -4.237966970562988323 ) ) ;
#17882 = ADVANCED_FACE ( 'NONE', ( #3118 ), #239, .T. ) ;
#17883 = CARTESIAN_POINT ( 'NONE',  ( -1.027846397803541700, 22.49680007765648071, 3.346150245485522312 ) ) ;
#17884 = ORIENTED_EDGE ( 'NONE', *, *, #15453, .F. ) ;
#17885 = LINE ( 'NONE', #5156, #16791 ) ;
#17886 = DIRECTION ( 'NONE',  ( -0.000000000000000000, 1.000000000000000000, -0.000000000000000000 ) ) ;
#17887 = FACE_OUTER_BOUND ( 'NONE', #7742, .T. ) ;
#17888 = AXIS2_PLACEMENT_3D ( 'NONE', #2683, #1289, #6920 ) ;
#17889 = CARTESIAN_POINT ( 'NONE',  ( 7.381366913268024632, -13.34886440523947648, 2.833380585799200269 ) ) ;
#17890 = CARTESIAN_POINT ( 'NONE',  ( 2.121784821875004390, -17.62046495959427261, -7.290387009954915953 ) ) ;
#17891 = ORIENTED_EDGE ( 'NONE', *, *, #16123, .T. ) ;
#17892 = CARTESIAN_POINT ( 'NONE',  ( 7.999999999999998224, 43.00000000000000000, -2.500000000000003109 ) ) ;
#17893 = CARTESIAN_POINT ( 'NONE',  ( 4.000000000000000888, -23.65828889131411827, -9.506058055638460402 ) ) ;
#17894 = CARTESIAN_POINT ( 'NONE',  ( 3.481649420246369697, 31.62180007765647360, -1.193696214020541824 ) ) ;
#17895 = ORIENTED_EDGE ( 'NONE', *, *, #11625, .T. ) ;
#17896 = VERTEX_POINT ( 'NONE', #1633 ) ;
#17897 = CARTESIAN_POINT ( 'NONE',  ( 3.999999999999996447, -28.15264258436690525, -11.89834241688737393 ) ) ;
#17898 = EDGE_CURVE ( 'NONE', #1108, #3470, #16927, .T. ) ;
#17899 = PRESENTATION_STYLE_ASSIGNMENT (( #16223 ) ) ;
#17900 = CARTESIAN_POINT ( 'NONE',  ( 3.673772985318163098, 30.50319992234354416, -2.599342558261029001 ) ) ;
#17901 = CARTESIAN_POINT ( 'NONE',  ( 1.071796769724494780, -26.92337036704631004, -7.195290474571613970 ) ) ;
#17902 = CARTESIAN_POINT ( 'NONE',  ( 0.8262555684460829442, 30.25319992234354771, -2.360188852285421302 ) ) ;
#17903 = EDGE_CURVE ( 'NONE', #17767, #17541, #145, .T. ) ;
#17904 = TOROIDAL_SURFACE ( 'NONE', #2201, 6.099999999999999645, 0.4000000000000000222 ) ;
#17905 = EDGE_LOOP ( 'NONE', ( #16271, #5211, #14695, #7863, #250 ) ) ;
#17906 = CARTESIAN_POINT ( 'NONE',  ( 1.336863392178479160, 23.74680007765647716, -4.297206761780677731 ) ) ;
#17907 = CARTESIAN_POINT ( 'NONE',  ( -3.999999999999997335, -19.52959017573017064, -7.635983121617017311 ) ) ;
#17908 = VERTEX_POINT ( 'NONE', #523 ) ;
#17909 = LINE ( 'NONE', #13709, #6202 ) ;
#17910 = AXIS2_PLACEMENT_3D ( 'NONE', #6211, #14760, #16237 ) ;
#17911 = CARTESIAN_POINT ( 'NONE',  ( -2.115076519116362519, 35.12180007765645939, 3.012182706137107147 ) ) ;
#17912 = DIRECTION ( 'NONE',  ( 0.000000000000000000, 0.000000000000000000, -1.000000000000000000 ) ) ;
#17913 = CARTESIAN_POINT ( 'NONE',  ( -4.243569643750004339, -22.23990597896245447, -3.208907214924944462 ) ) ;
#17914 = CARTESIAN_POINT ( 'NONE',  ( -2.121784821874996396, -21.44908767223746437, -12.75822690558396033 ) ) ;
#17915 = PRODUCT_DEFINITION_SHAPE ( 'NONE', 'NONE',  #18372 ) ;
#17916 = CARTESIAN_POINT ( 'NONE',  ( 0.000000000000000000, 5.977523610840987267, 32.81826849749789687 ) ) ;
#17917 = ORIENTED_EDGE ( 'NONE', *, *, #3203, .T. ) ;
#17918 = CARTESIAN_POINT ( 'NONE',  ( 4.898587196589417759E-16, -3.999999999999993339, 25.54267522293723758 ) ) ;
#17919 = CARTESIAN_POINT ( 'NONE',  ( 2.211161402132902243, 17.12180007765647360, 2.942372952327172442 ) ) ;
#17920 = CARTESIAN_POINT ( 'NONE',  ( -2.121784821875005722, -29.44875798415262835, -11.36846978121561236 ) ) ;
#17921 = VERTEX_POINT ( 'NONE', #17226 ) ;
#17922 = CARTESIAN_POINT ( 'NONE',  ( -3.481649420246394122, 34.62819992234354771, -1.193696214020467883 ) ) ;
#17923 = FACE_BOUND ( 'NONE', #6204, .T. ) ;
#17924 = EDGE_CURVE ( 'NONE', #10194, #1083, #5795, .T. ) ;
#17925 = CARTESIAN_POINT ( 'NONE',  ( 4.243569643750003451, -18.09696354311409294, -5.835152456403505106 ) ) ;
#17926 = CARTESIAN_POINT ( 'NONE',  ( 0.8262555684461332373, 32.24680007765648071, 2.360188852285403982 ) ) ;
#17927 = CARTESIAN_POINT ( 'NONE',  ( -2.733110507866328476, 22.37819992234354416, -3.862833514489096398 ) ) ;
#17928 = UNCERTAINTY_MEASURE_WITH_UNIT (LENGTH_MEASURE( 1.000000000000000082E-05 ), #7948, 'distance_accuracy_value', 'NONE');
#17929 = CARTESIAN_POINT ( 'NONE',  ( 1.999999999999994449, -28.02306207205872113, -9.700123312982540824 ) ) ;
#17930 = ORIENTED_EDGE ( 'NONE', *, *, #8391, .T. ) ;
#17931 = CARTESIAN_POINT ( 'NONE',  ( -2.121784821875005722, -22.73791367884544812, -1.784390863034371666 ) ) ;
#17932 = CARTESIAN_POINT ( 'NONE',  ( -2.211161402132902243, 15.87180007765647716, -2.942372952327172886 ) ) ;
#17933 = CARTESIAN_POINT ( 'NONE',  ( 8.673617379884035472E-15, 13.00000000000000178, 3.469446951953614189E-15 ) ) ;
#17934 = CARTESIAN_POINT ( 'NONE',  ( 4.243569643750003451, -21.96860448848362779, -11.36442875535422026 ) ) ;
#17935 = DIRECTION ( 'NONE',  ( 0.000000000000000000, 0.000000000000000000, 1.000000000000000000 ) ) ;
#17936 = CARTESIAN_POINT ( 'NONE',  ( 1.071796769724494780, -27.69769855612021558, -8.301145734361757178 ) ) ;
#17937 = DIRECTION ( 'NONE',  ( -0.000000000000000000, -1.000000000000000000, -0.000000000000000000 ) ) ;
#17938 = ORIENTED_EDGE ( 'NONE', *, *, #4651, .F. ) ;
#17939 = ORIENTED_EDGE ( 'NONE', *, *, #15453, .T. ) ;
#17940 = CARTESIAN_POINT ( 'NONE',  ( 3.518350579753631191, 19.37180007765648071, 1.080741659609802285 ) ) ;
#17941 = CARTESIAN_POINT ( 'NONE',  ( 1.999999999999994449, -24.47405787284159828, -4.631620039951150680 ) ) ;
#17942 = CARTESIAN_POINT ( 'NONE',  ( 7.343428405759329536, -12.39714631489042418, 9.301343483023684300 ) ) ;
#17943 = ORIENTED_EDGE ( 'NONE', *, *, #8797, .T. ) ;
#17944 = CARTESIAN_POINT ( 'NONE',  ( 1.989345975306457071, 36.00319992234354771, 1.515154207786300500 ) ) ;
#17945 = APPLICATION_PROTOCOL_DEFINITION ( 'draft international standard', 'automotive_design', 1998, #15786 ) ;
#17946 = CARTESIAN_POINT ( 'NONE',  ( -4.243569643749997233, -21.62445862667299323, -10.87293752878082742 ) ) ;
#17947 = CARTESIAN_POINT ( 'NONE',  ( -2.864755990943265829, 28.24680007765648071, -2.011557305968488141 ) ) ;
#17948 = CARTESIAN_POINT ( 'NONE',  ( -0.05938372350920063936, 16.37819992234354416, 3.680117784833935701 ) ) ;
#17949 = CARTESIAN_POINT ( 'NONE',  ( 8.000000000000000000, 43.00000000000000000, -2.500000000000000888 ) ) ;
#17950 = DIRECTION ( 'NONE',  ( 0.000000000000000000, -0.5735764363510567065, -0.8191520442889842490 ) ) ;
#17951 = CARTESIAN_POINT ( 'NONE',  ( 2.121784821875004390, -21.23399650860583066, -12.45104488897558248 ) ) ;
#17952 = ADVANCED_FACE ( 'NONE', ( #4407 ), #10048, .F. ) ;
#17953 = EDGE_CURVE ( 'NONE', #2204, #13322, #4500, .T. ) ;
#17954 = CARTESIAN_POINT ( 'NONE',  ( -1.734723475976807094E-15, 20.99999999999999289, -2.500000000000000000 ) ) ;
#17955 = CARTESIAN_POINT ( 'NONE',  ( -3.607379964056306676, 22.74680007765647716, 2.690724712371306282 ) ) ;
#17956 = ADVANCED_FACE ( 'NONE', ( #14906 ), #620, .F. ) ;
#17957 = DIRECTION ( 'NONE',  ( 0.000000000000000000, -1.000000000000000000, 0.000000000000000000 ) ) ;
#17958 = DIRECTION ( 'NONE',  ( 0.000000000000000000, 0.000000000000000000, -1.000000000000000000 ) ) ;
#17959 = CARTESIAN_POINT ( 'NONE',  ( -5.330712181944245322E-15, -26.26870678593457242, -4.691140945321855327 ) ) ;
#17960 = CIRCLE ( 'NONE', #16484, 4.400000000000002132 ) ;
#17961 = ORIENTED_EDGE ( 'NONE', *, *, #15547, .F. ) ;
#17962 = FACE_BOUND ( 'NONE', #11730, .T. ) ;
#17963 = DIRECTION ( 'NONE',  ( -0.000000000000000000, -0.5735764363510414965, -0.8191520442889950182 ) ) ;
#17964 = EDGE_CURVE ( 'NONE', #13832, #3421, #7917, .T. ) ;
#17965 = CARTESIAN_POINT ( 'NONE',  ( 2.518350579753628971, 36.87180007765648071, 0.7558219633769073242 ) ) ;
#17966 = CARTESIAN_POINT ( 'NONE',  ( -9.000000000000001776, 29.79999999999999716, 2.499999999999995559 ) ) ;
#17967 = CARTESIAN_POINT ( 'NONE',  ( -1.027846397803541700, 37.49680007765647360, 3.346150245485522312 ) ) ;
#17968 = CARTESIAN_POINT ( 'NONE',  ( -3.999999999999997335, -23.40123112109970194, -13.16525942056773424 ) ) ;
#17969 = SHAPE_DEFINITION_REPRESENTATION ( #10476, #5306 ) ;
#17970 = CARTESIAN_POINT ( 'NONE',  ( -3.052806949544935478, 15.00000000000000888, -2.471371977836584133 ) ) ;
#17971 = ADVANCED_FACE ( 'NONE', ( #5048 ), #9399, .F. ) ;
#17972 = ORIENTED_EDGE ( 'NONE', *, *, #6834, .T. ) ;
#17973 = CARTESIAN_POINT ( 'NONE',  ( -4.243569643750004339, -23.82082603165501666, -5.466695036996486401 ) ) ;
#17974 = UNCERTAINTY_MEASURE_WITH_UNIT (LENGTH_MEASURE( 1.000000000000000082E-05 ), #16959, 'distance_accuracy_value', 'NONE');
#17975 = CARTESIAN_POINT ( 'NONE',  ( -2.211161402132902243, 20.87180007765647716, -2.942372952327172886 ) ) ;
#17976 = ORIENTED_EDGE ( 'NONE', *, *, #15843, .F. ) ;
#17977 = DIRECTION ( 'NONE',  ( 0.000000000000000000, 0.000000000000000000, 1.000000000000000000 ) ) ;
#17978 = CIRCLE ( 'NONE', #11144, 6.000000000000000888 ) ;
#17979 = DIRECTION ( 'NONE',  ( 0.000000000000000000, -1.000000000000000000, 0.000000000000000000 ) ) ;
#17980 = CARTESIAN_POINT ( 'NONE',  ( 1.005564577543283766, -23.86805906247938935, -16.73400458965339865 ) ) ;
#17981 = CARTESIAN_POINT ( 'NONE',  ( 9.000000000000005329, -10.00000000000000178, -3.713574246709346216 ) ) ;
#17982 = CARTESIAN_POINT ( 'NONE',  ( 4.000000000000000888, -24.62619912695155477, -10.88837712936937230 ) ) ;
#17983 = CARTESIAN_POINT ( 'NONE',  ( 4.730628863548789710E-15, -21.72540816142837983, -15.28859851726467589 ) ) ;
#17984 = ORIENTED_EDGE ( 'NONE', *, *, #12476, .T. ) ;
#17985 = DIRECTION ( 'NONE',  ( -0.000000000000000000, -1.000000000000000000, 1.502314598737159031E-16 ) ) ;
#17986 = CARTESIAN_POINT ( 'NONE',  ( 4.713407268011036227E-15, -17.48727574878303770, -8.745573750710319061 ) ) ;
#17987 = CARTESIAN_POINT ( 'NONE',  ( -2.500000000000001332, 15.49680007765647893, 0.05647727720535858364 ) ) ;
#17988 = VERTEX_POINT ( 'NONE', #7737 ) ;
#17989 = EDGE_LOOP ( 'NONE', ( #14971, #2956, #16975, #2112, #15305 ) ) ;
#17990 = CARTESIAN_POINT ( 'NONE',  ( -4.000000000000004441, -23.01196377286574091, -4.556692218940494143 ) ) ;
#17991 =( NAMED_UNIT ( * ) PLANE_ANGLE_UNIT ( ) SI_UNIT ( $, .RADIAN. ) );
#17992 = CARTESIAN_POINT ( 'NONE',  ( -3.607379964056363075, 34.75319992234354771, -2.690724712371229899 ) ) ;
#17993 = DIRECTION ( 'NONE',  ( 1.000000000000000000, 0.000000000000000000, 0.000000000000000000 ) ) ;
#17994 = CIRCLE ( 'NONE', #1102, 0.4000000000000001887 ) ;
#17995 = CARTESIAN_POINT ( 'NONE',  ( -0.8262555684460826111, 29.00319992234355482, 2.360188852285421302 ) ) ;
#17996 = ORIENTED_EDGE ( 'NONE', *, *, #5856, .F. ) ;
#17997 = CARTESIAN_POINT ( 'NONE',  ( -4.243569643750000786, -25.70703222455301784, -12.43196676332983408 ) ) ;
#17998 = CARTESIAN_POINT ( 'NONE',  ( -3.607379964056306676, 25.24680007765648071, 2.690724712371306282 ) ) ;
#17999 = CARTESIAN_POINT ( 'NONE',  ( 3.999999999999996447, -22.15159911833918827, -3.327964152506997397 ) ) ;
#18000 = ORIENTED_EDGE ( 'NONE', *, *, #947, .T. ) ;
#18001 = DIRECTION ( 'NONE',  ( -1.000000000000000000, 0.000000000000000000, 4.336808689942021680E-16 ) ) ;
#18002 =( NAMED_UNIT ( * ) PLANE_ANGLE_UNIT ( ) SI_UNIT ( $, .RADIAN. ) );
#18003 =( BOUNDED_CURVE ( )  B_SPLINE_CURVE ( 2, ( #1433, #12451, #8541, #9761, #16929 ),
 .UNSPECIFIED., .F., .T. ) 
 B_SPLINE_CURVE_WITH_KNOTS ( ( 3, 2, 3 ),
 ( 0.004713559543201377953, 0.005747126436781609116, 0.008620689655172418878 ),
 .UNSPECIFIED. ) 
 CURVE ( )  GEOMETRIC_REPRESENTATION_ITEM ( )  RATIONAL_B_SPLINE_CURVE ( ( 0.9604780343359251571, 0.9759059229421220838, 1.000000000000000000, 0.9330127018922191873, 0.9330127018922192983 ) ) 
 REPRESENTATION_ITEM ( '' )  );
#18004 = CARTESIAN_POINT ( 'NONE',  ( 9.000000000000000000, 29.79999999999999716, -2.500000000000001332 ) ) ;
#18005 = CARTESIAN_POINT ( 'NONE',  ( -4.243569643750000786, -20.51258062284889760, -5.013521062237622949 ) ) ;
#18006 = TOROIDAL_SURFACE ( 'NONE', #9966, 9.000000000000003553, 0.9999999999999991118 ) ;
#18007 = CARTESIAN_POINT ( 'NONE',  ( -5.330712181944245322E-15, -26.55907985683728967, -5.105836667743160362 ) ) ;
#18008 = CARTESIAN_POINT ( 'NONE',  ( -8.000000000000003553, 29.79999999999999716, -2.500000000000001776 ) ) ;
#18009 = EDGE_LOOP ( 'NONE', ( #291, #12118 ) ) ;
#18010 = CARTESIAN_POINT ( 'NONE',  ( -1.999999999999996225, -21.50895469527046444, -12.47596756835385534 ) ) ;
#18011 = CARTESIAN_POINT ( 'NONE',  ( -9.000000000000001776, 18.79999999999999361, 2.499999999999995559 ) ) ;
#18012 = EDGE_LOOP ( 'NONE', ( #5665, #8488, #13673, #15854 ) ) ;
#18013 = CARTESIAN_POINT ( 'NONE',  ( -2.864755990943222308, 36.75319992234354061, 2.011557305968548093 ) ) ;
#18014 = CARTESIAN_POINT ( 'NONE',  ( -3.500000000000000444, 19.50319992234354416, -0.05647727720529563400 ) ) ;
#18015 = CARTESIAN_POINT ( 'NONE',  ( -4.000000000000000888, -26.88465634578871999, -14.11378830476406065 ) ) ;
#18016 = CARTESIAN_POINT ( 'NONE',  ( 0.7188294034286049072, 31.24680007765648071, -2.395093729190366005 ) ) ;
#18017 = VECTOR ( 'NONE', #15566, 1000.000000000000000 ) ;
#18018 = CARTESIAN_POINT ( 'NONE',  ( 2.829195390882724759, 22.87819992234354416, -3.793023760679264278 ) ) ;
#18019 = AXIS2_PLACEMENT_3D ( 'NONE', #2378, #6708, #706 ) ;
#18020 = CARTESIAN_POINT ( 'NONE',  ( 4.713407268011036227E-15, -21.55249874071609995, -14.55131386360180734 ) ) ;
#18021 = ORIENTED_EDGE ( 'NONE', *, *, #11576, .T. ) ;
#18022 = CARTESIAN_POINT ( 'NONE',  ( 2.121784821874994176, -23.21111423883506220, -2.460191299572788814 ) ) ;
#18023 = CARTESIAN_POINT ( 'NONE',  ( -4.499999999999999112, 35.49680007765647360, 0.05647727720537927543 ) ) ;
#18024 = DIRECTION ( 'NONE',  ( -0.000000000000000000, 1.000000000000000000, -0.000000000000000000 ) ) ;
#18025 = CARTESIAN_POINT ( 'NONE',  ( -4.243569643750000786, -24.38422156821842535, -10.54279736118833988 ) ) ;
#18026 = EDGE_CURVE ( 'NONE', #13741, #12298, #6250, .T. ) ;
#18027 = CLOSED_SHELL ( 'NONE', ( #16757, #5476, #9554, #11218, #11018, #6713, #9370, #11678, #7391, #13866, #12992, #3953, #5416, #2317, #5691, #12250, #15067, #17001, #2322, #4185, #5578, #7521, #7363, #2749, #15114, #4674, #4789 ) ) ;
#18028 = CARTESIAN_POINT ( 'NONE',  ( -3.999999999999997335, -18.75526198665626154, -6.530127861826874103 ) ) ;
#18029 = MECHANICAL_DESIGN_GEOMETRIC_PRESENTATION_REPRESENTATION (  '', ( #9693 ), #1731 ) ;
#18030 = DIRECTION ( 'NONE',  ( 1.000000000000000000, 0.000000000000000000, -4.336808689942021680E-16 ) ) ;
#18031 = VECTOR ( 'NONE', #2972, 1000.000000000000000 ) ;
#18032 = ORIENTED_EDGE ( 'NONE', *, *, #11863, .F. ) ;
#18033 = CIRCLE ( 'NONE', #13266, 0.9999999999999991118 ) ;
#18034 = ORIENTED_EDGE ( 'NONE', *, *, #13676, .T. ) ;
#18035 = FACE_OUTER_BOUND ( 'NONE', #13071, .T. ) ;
#18036 = DIRECTION ( 'NONE',  ( 0.000000000000000000, 0.000000000000000000, -1.000000000000000000 ) ) ;
#18037 = DIRECTION ( 'NONE',  ( 3.469446951953612217E-16, -0.000000000000000000, 1.000000000000000000 ) ) ;
#18038 = CARTESIAN_POINT ( 'NONE',  ( 4.000000000000003553, -24.00348637926830264, -14.02536906707117659 ) ) ;
#18039 = ORIENTED_EDGE ( 'NONE', *, *, #8391, .F. ) ;
#18040 = CARTESIAN_POINT ( 'NONE',  ( 2.055738996568281518, 35.50319992234354771, -1.423772053676066518 ) ) ;
#18041 = CARTESIAN_POINT ( 'NONE',  ( -4.243569643750005227, -26.11154692433198576, -8.738183513875661390 ) ) ;
#18042 = CARTESIAN_POINT ( 'NONE',  ( 1.027846397803542144, 28.74680007765647716, -3.346150245485522312 ) ) ;
#18043 = CARTESIAN_POINT ( 'NONE',  ( -3.481649420246394122, 29.62819992234353350, -1.193696214020467883 ) ) ;
#18044 = PLANE ( 'NONE',  #9585 ) ;
#18045 = DIRECTION ( 'NONE',  ( 1.000000000000000000, 0.000000000000000000, 0.000000000000000000 ) ) ;
#18046 = AXIS2_PLACEMENT_3D ( 'NONE', #17966, #12458, #9590 ) ;
#18047 = AXIS2_PLACEMENT_3D ( 'NONE', #5488, #6515, #13742 ) ;
#18048 = CARTESIAN_POINT ( 'NONE',  ( 4.243569643749996345, -26.57399292614002562, -9.398624849583658403 ) ) ;
#18049 = AXIS2_PLACEMENT_3D ( 'NONE', #17084, #4546, #14287 ) ;
#18050 = CARTESIAN_POINT ( 'NONE',  ( 9.000000000000000000, 23.19999999999999574, -2.500000000000001332 ) ) ;
#18051 = CARTESIAN_POINT ( 'NONE',  ( -4.499999999999999112, 20.49680007765647716, 0.05647727720537927543 ) ) ;
#18052 = DIRECTION ( 'NONE',  ( 0.000000000000000000, 0.000000000000000000, -1.000000000000000000 ) ) ;
#18053 = CIRCLE ( 'NONE', #13587, 10.00000000000000000 ) ;
#18054 = CARTESIAN_POINT ( 'NONE',  ( 3.579096709490575479E-14, -25.90245948233327056, -5.737278629507336802 ) ) ;
#18055 = CARTESIAN_POINT ( 'NONE',  ( -2.121784821874996396, -19.61005822318693248, -10.13182066358236888 ) ) ;
#18056 = FACE_OUTER_BOUND ( 'NONE', #10084, .T. ) ;
#18057 = CARTESIAN_POINT ( 'NONE',  ( 10.00000000000000355, 20.99999999999999289, 2.499999999999996891 ) ) ;
#18058 = AXIS2_PLACEMENT_3D ( 'NONE', #16395, #17531, #17709 ) ;
#18059 = CARTESIAN_POINT ( 'NONE',  ( -1.497042530366477164, 37.62180007765646650, 2.161531897785062384 ) ) ;
#18060 = CARTESIAN_POINT ( 'NONE',  ( -9.000000000000001776, 25.39999999999999503, 2.499999999999998224 ) ) ;
#18061 = CARTESIAN_POINT ( 'NONE',  ( -2.798362969681365886, 40.24680007765648071, 2.102939460078824929 ) ) ;
#18062 = CARTESIAN_POINT ( 'NONE',  ( 8.500000000000001776, 15.00000000000000178, -22.64999999999999147 ) ) ;
#18063 = EDGE_CURVE ( 'NONE', #1200, #3107, #10401, .T. ) ;
#18064 = CARTESIAN_POINT ( 'NONE',  ( -4.000000000000000000, 15.00000000000000355, 4.083367561434192880E-14 ) ) ;
#18065 = EDGE_LOOP ( 'NONE', ( #7946, #11792, #6917, #8524 ) ) ;
#18066 = CARTESIAN_POINT ( 'NONE',  ( 4.243569643750000786, -21.96444597736247673, -7.086999674344137468 ) ) ;
#18067 = CARTESIAN_POINT ( 'NONE',  ( 2.211161402132902243, 24.62180007765647716, 2.942372952327172442 ) ) ;
#18068 = CIRCLE ( 'NONE', #2665, 1.250000000000000222 ) ;
#18069 = DIRECTION ( 'NONE',  ( -4.915049848600951133E-16, 0.000000000000000000, -1.000000000000000000 ) ) ;
#18070 = AXIS2_PLACEMENT_3D ( 'NONE', #13348, #6303, #11857 ) ;
#18071 = CARTESIAN_POINT ( 'NONE',  ( 4.243569643750000786, -26.57815143726116602, -13.67605393059374208 ) ) ;
#18072 = CARTESIAN_POINT ( 'NONE',  ( -4.036928234951689731, -26.90731100780323715, -14.49060178547057021 ) ) ;
#18073 = CARTESIAN_POINT ( 'NONE',  ( 1.071796769724495224, -23.10335607593069440, -15.68731904395727739 ) ) ;
#18074 = DIRECTION ( 'NONE',  ( -0.000000000000000000, -1.000000000000000000, -0.000000000000000000 ) ) ;
#18075 = CARTESIAN_POINT ( 'NONE',  ( 2.121784821874994176, -29.11536668052359289, -10.89233765547263211 ) ) ;
#18076 = VERTEX_POINT ( 'NONE', #3484 ) ;
#18077 = CARTESIAN_POINT ( 'NONE',  ( -4.000000000000000888, -23.72281623969865905, -9.598212659614208775 ) ) ;
#18078 = ADVANCED_FACE ( 'NONE', ( #3668 ), #7641, .F. ) ;
#18079 = CARTESIAN_POINT ( 'NONE',  ( -2.000000000000005773, -24.00085731285198065, -3.955819603412733976 ) ) ;
#18080 = CARTESIAN_POINT ( 'NONE',  ( -1.027846397803541700, 39.99680007765648071, 3.346150245485522312 ) ) ;
#18081 = VERTEX_POINT ( 'NONE', #6443 ) ;
#18082 = CARTESIAN_POINT ( 'NONE',  ( 4.000000000000003553, -23.55179493634679844, -13.38028683320035661 ) ) ;
#18083 = EDGE_CURVE ( 'NONE', #17611, #2412, #2014, .T. ) ;
#18084 = AXIS2_PLACEMENT_3D ( 'NONE', #11065, #4114, #16930 ) ;
#18085 = CARTESIAN_POINT ( 'NONE',  ( -2.733110507866328476, 34.87819992234354771, -3.862833514489096398 ) ) ;
#18086 = UNCERTAINTY_MEASURE_WITH_UNIT (LENGTH_MEASURE( 1.000000000000000082E-05 ), #109, 'distance_accuracy_value', 'NONE');
#18087 = CARTESIAN_POINT ( 'NONE',  ( -1.071796769724496334, -23.59100161583038613, -2.436174684792825396 ) ) ;
#18089 = ADVANCED_FACE ( 'NONE', ( #6532 ), #2432, .T. ) ;
#18088 = COLOUR_RGB ( '',0.8941176470588234615, 0.8941176470588234615, 0.8941176470588234615 ) ;
#18090 = CARTESIAN_POINT ( 'NONE',  ( -0.05938372350921170689, 31.37819992234354061, 2.628655560595669183 ) ) ;
#18091 = EDGE_LOOP ( 'NONE', ( #14910, #7051, #1837, #12775 ) ) ;
#18092 = CARTESIAN_POINT ( 'NONE',  ( 4.243569643750003451, -23.03330574846025058, -12.88497973756566672 ) ) ;
#18093 = CARTESIAN_POINT ( 'NONE',  ( 3.673772985318219053, 21.99680007765647716, 2.599342558260951730 ) ) ;
#18094 = CARTESIAN_POINT ( 'NONE',  ( 1.999999999999994449, -23.37709293761528784, -3.064991754241682465 ) ) ;
#18095 = ORIENTED_EDGE ( 'NONE', *, *, #813, .F. ) ;
#18096 = DIRECTION ( 'NONE',  ( 1.000000000000000000, 0.000000000000000000, -0.000000000000000000 ) ) ;
#18097 = CARTESIAN_POINT ( 'NONE',  ( 0.000000000000000000, 43.00000000000000000, -6.499999999999999112 ) ) ;
#18098 = LINE ( 'NONE', #9804, #16094 ) ;
#18099 = MECHANICAL_DESIGN_GEOMETRIC_PRESENTATION_REPRESENTATION (  '', ( #5411 ), #17339 ) ;
#18100 = CIRCLE ( 'NONE', #8889, 4.400000000000002132 ) ;
#18101 = DIRECTION ( 'NONE',  ( 1.000000000000000000, 0.000000000000000000, 0.000000000000000000 ) ) ;
#18102=STYLED_ITEM('',(#18396),#7707);
#18103 = CARTESIAN_POINT ( 'NONE',  ( 2.121784821874994176, -25.53409880605677884, -5.777757078943218438 ) ) ;
#18104 = DIRECTION ( 'NONE',  ( 0.000000000000000000, 0.000000000000000000, 1.000000000000000000 ) ) ;
#18105 = ORIENTED_EDGE ( 'NONE', *, *, #314, .T. ) ;
#18106 = CARTESIAN_POINT ( 'NONE',  ( 4.000000000000003553, -22.00313855819898734, -11.16857631362007020 ) ) ;
#18107 = DIRECTION ( 'NONE',  ( 0.000000000000000000, 0.000000000000000000, 1.000000000000000000 ) ) ;
#18108 = FACE_OUTER_BOUND ( 'NONE', #7392, .T. ) ;
#18109 = ORIENTED_EDGE ( 'NONE', *, *, #8299, .F. ) ;
#18110 = CARTESIAN_POINT ( 'NONE',  ( 1.135272562821020070, 32.75319992234354771, -3.311245368580577164 ) ) ;
#18111 = CARTESIAN_POINT ( 'NONE',  ( -2.115076519116425580, 19.87819992234354416, -3.012182706137063182 ) ) ;
#18112 = CARTESIAN_POINT ( 'NONE',  ( 4.243569643750000786, -20.64163532102788778, -5.197830272202643265 ) ) ;
#18113 = CARTESIAN_POINT ( 'NONE',  ( 2.481649420246374138, 26.62180007765648426, -0.8687765177876252132 ) ) ;
#18114 = VECTOR ( 'NONE', #8752, 1000.000000000000000 ) ;
#18115 = CARTESIAN_POINT ( 'NONE',  ( -4.481649420246396787, 22.12819992234354416, -1.518615910253363399 ) ) ;
#18116 = UNCERTAINTY_MEASURE_WITH_UNIT (LENGTH_MEASURE( 1.000000000000000082E-05 ), #6927, 'distance_accuracy_value', 'NONE');
#18117 = CARTESIAN_POINT ( 'NONE',  ( -1.999999999999996225, -21.44442734547602569, -12.38381296236458162 ) ) ;
#18118 =( BOUNDED_CURVE ( )  B_SPLINE_CURVE ( 2, ( #10778, #12346, #2455, #1057, #17770, #13746, #7898, #16548, #5121 ),
 .UNSPECIFIED., .F., .T. ) 
 B_SPLINE_CURVE_WITH_KNOTS ( ( 3, 2, 2, 2, 3 ),
 ( 0.4051724137931034808, 0.4080459770114942541, 0.4137931034482758563, 0.4195402298850574585, 0.4224137931034482873 ),
 .UNSPECIFIED. ) 
 CURVE ( )  GEOMETRIC_REPRESENTATION_ITEM ( )  RATIONAL_B_SPLINE_CURVE ( ( 0.9330127018922194093, 0.9330127018922200755, 1.000000000000000000, 0.8660254037844387076, 1.000000000000000000, 0.8660254037844387076, 1.000000000000000000, 0.9330127018922187432, 0.9330127018922194093 ) ) 
 REPRESENTATION_ITEM ( '' )  );
#18119 = VERTEX_POINT ( 'NONE', #11911 ) ;
#18120 = CARTESIAN_POINT ( 'NONE',  ( 4.243569643750003451, -18.38733661401680308, -6.249848178824808365 ) ) ;
#18121 = CARTESIAN_POINT ( 'NONE',  ( -0.05938372350927861171, 21.12180007765648071, -3.680117784833935701 ) ) ;
#18122 = DIRECTION ( 'NONE',  ( -0.000000000000000000, -0.5735764363510414965, -0.8191520442889950182 ) ) ;
#18123 = CARTESIAN_POINT ( 'NONE',  ( -2.121784821874996396, -19.35194882682896633, -9.763202243652322920 ) ) ;
#18124 = CARTESIAN_POINT ( 'NONE',  ( 4.299564228933482956E-15, -23.09182937521185863, -15.67085720930136006 ) ) ;
#18125 = PRESENTATION_LAYER_ASSIGNMENT (  '', '', ( #42 ) ) ;
#18126 = CARTESIAN_POINT ( 'NONE',  ( -5.577813053751546416E-15, -24.67643985033786791, -3.986341135846375838 ) ) ;
#18127 = CARTESIAN_POINT ( 'NONE',  ( 9.000000000000005329, 20.99999999999999289, 2.499999999999997335 ) ) ;
#18128 = ORIENTED_EDGE ( 'NONE', *, *, #342, .F. ) ;
#18129 = ORIENTED_EDGE ( 'NONE', *, *, #13411, .T. ) ;
#18130 = CARTESIAN_POINT ( 'NONE',  ( 1.027846397803542144, 18.74680007765648071, -3.346150245485522312 ) ) ;
#18131 = CARTESIAN_POINT ( 'NONE',  ( 5.810221930991194676E-16, -23.67257551772223678, -16.50024865515073458 ) ) ;
#18132 = EDGE_CURVE ( 'NONE', #14859, #4548, #17693, .T. ) ;
#18133 = CARTESIAN_POINT ( 'NONE',  ( 1.071796769724487675, -30.08521047313637453, -11.71086611972146407 ) ) ;
#18134 = DIRECTION ( 'NONE',  ( -1.000000000000000000, 0.000000000000000000, 0.000000000000000000 ) ) ;
#18135 = ORIENTED_EDGE ( 'NONE', *, *, #11135, .F. ) ;
#18136 = CARTESIAN_POINT ( 'NONE',  ( -0.05938372350921170689, 38.87819992234354771, 2.628655560595669183 ) ) ;
#18137 = CARTESIAN_POINT ( 'NONE',  ( -4.243569643750000786, -24.64233096457639505, -10.91141578111838584 ) ) ;
#18138 = CARTESIAN_POINT ( 'NONE',  ( 0.05938372350927906274, 32.37180007765647360, 3.680117784833935701 ) ) ;
#18139 = EDGE_CURVE ( 'NONE', #16136, #7494, #10703, .T. ) ;
#18140 = CARTESIAN_POINT ( 'NONE',  ( 2.211161402132839626, 25.37819992234353705, -2.942372952327218183 ) ) ;
#18141 = FACE_OUTER_BOUND ( 'NONE', #15103, .T. ) ;
#18142 = ADVANCED_FACE ( 'NONE', ( #11999 ), #17549, .T. ) ;
#18143 = CARTESIAN_POINT ( 'NONE',  ( 0.000000000000000000, -2.372474330222551941, 20.89323558166710626 ) ) ;
#18144 = PRESENTATION_LAYER_ASSIGNMENT (  '', '', ( #10995 ) ) ;
#18145 = CARTESIAN_POINT ( 'NONE',  ( -4.243569643749997233, -21.65672230121773723, -10.91901483127208294 ) ) ;
#18146 = DIRECTION ( 'NONE',  ( -1.000000000000000000, 0.000000000000000000, 4.336808689942021680E-16 ) ) ;
#18147 = CIRCLE ( 'NONE', #5966, 3.047499999999999876 ) ;
#18148 = DIRECTION ( 'NONE',  ( -0.000000000000000000, -1.000000000000000000, -0.000000000000000000 ) ) ;
#18149 = CARTESIAN_POINT ( 'NONE',  ( -2.121784821874996396, -18.57762063775506078, -8.657346983862177936 ) ) ;
#18150 = CARTESIAN_POINT ( 'NONE',  ( -1.071796769724494114, -30.04373652477960732, -11.65163518304401613 ) ) ;
#18151 = DIRECTION ( 'NONE',  ( 0.8191520442889951292, 0.4698463103929522156, -0.3289899283371602867 ) ) ;
#18152 = CARTESIAN_POINT ( 'NONE',  ( 2.055738996568313048, 39.49680007765648071, 1.423772053676023441 ) ) ;
#18153 = DIRECTION ( 'NONE',  ( 0.000000000000000000, 0.000000000000000000, 1.000000000000000000 ) ) ;
#18154 = CARTESIAN_POINT ( 'NONE',  ( -2.211161402132901799, 38.37180007765647360, -2.942372952327172886 ) ) ;
#18155 = CARTESIAN_POINT ( 'NONE',  ( -1.165965068879164734, 15.00000000000001421, -3.401582918303170278 ) ) ;
#18156 = EDGE_CURVE ( 'NONE', #15490, #3198, #9508, .T. ) ;
#18157 = EDGE_LOOP ( 'NONE', ( #5692, #2233, #3562 ) ) ;
#18158 = AXIS2_PLACEMENT_3D ( 'NONE', #8757, #12846, #1638 ) ;
#18159 = CARTESIAN_POINT ( 'NONE',  ( 2.121784821875004390, -18.65290254502614431, -8.764860689675106897 ) ) ;
#18160 = CARTESIAN_POINT ( 'NONE',  ( 0.05938372350927906274, 24.87180007765647005, 3.680117784833935701 ) ) ;
#18161 = CIRCLE ( 'NONE', #6575, 2.149999999999995470 ) ;
#18162 = CARTESIAN_POINT ( 'NONE',  ( 8.500000000000019540, 10.00000000000000000, -20.49999999999998934 ) ) ;
#18163 = FACE_OUTER_BOUND ( 'NONE', #19, .T. ) ;
#18164 = CARTESIAN_POINT ( 'NONE',  ( -8.500000000000005329, 0.000000000000000000, -20.49999999999999645 ) ) ;
#18165 = CARTESIAN_POINT ( 'NONE',  ( 8.673617379884035472E-16, 0.000000000000000000, 0.000000000000000000 ) ) ;
#18166 = CARTESIAN_POINT ( 'NONE',  ( 0.000000000000000000, 0.000000000000000000, 2.000000000000000000 ) ) ;
#18167 = CARTESIAN_POINT ( 'NONE',  ( -4.243569643750000786, -26.19098734272420614, -13.12312630069867225 ) ) ;
#18168 = EDGE_LOOP ( 'NONE', ( #4739, #14793, #17697 ) ) ;
#18169 = CARTESIAN_POINT ( 'NONE',  ( -1.734723475976807094E-15, 31.99999999999999289, -2.500000000000000000 ) ) ;
#18170 = VECTOR ( 'NONE', #13451, 1000.000000000000000 ) ;
#18171 = CARTESIAN_POINT ( 'NONE',  ( -2.000000000000005773, -24.51707610556791650, -4.693056443272829448 ) ) ;
#18172 = AXIS2_PLACEMENT_3D ( 'NONE', #10363, #16043, #3336 ) ;
#18173 = CARTESIAN_POINT ( 'NONE',  ( -0.05938372350926768989, 16.12180007765648071, -2.628655560595669183 ) ) ;
#18174 = ORIENTED_EDGE ( 'NONE', *, *, #7259, .F. ) ;
#18175 = CARTESIAN_POINT ( 'NONE',  ( -12.99999999999999822, 13.00000000000000178, 0.000000000000000000 ) ) ;
#18176 = CARTESIAN_POINT ( 'NONE',  ( -4.481649420246366589, 17.87180007765647360, 1.518615910253458878 ) ) ;
#18177 = PLANE ( 'NONE',  #11618 ) ;
#18178 = CARTESIAN_POINT ( 'NONE',  ( 0.8262555684460829442, 27.75319992234355126, -2.360188852285421302 ) ) ;
#18179 = VERTEX_POINT ( 'NONE', #3575 ) ;
#18180 = CARTESIAN_POINT ( 'NONE',  ( 4.730628863548789710E-15, -21.24145304325719152, -14.59743897989583594 ) ) ;
#18181 = CARTESIAN_POINT ( 'NONE',  ( 1.444289557196047680, 22.24680007765647716, 4.262301884875704161 ) ) ;
#18182 = CARTESIAN_POINT ( 'NONE',  ( 3.999999999999996447, -22.66781791105512767, -4.065200992367092425 ) ) ;
#18183 = ORIENTED_EDGE ( 'NONE', *, *, #10523, .T. ) ;
#18184 = AXIS2_PLACEMENT_3D ( 'NONE', #4594, #9882, #7097 ) ;
#18185 = CARTESIAN_POINT ( 'NONE',  ( 0.000000000000000000, 43.00000000000000000, 2.500000000000000000 ) ) ;
#18186 = TOROIDAL_SURFACE ( 'NONE', #4835, 9.000000000000001776, 0.9999999999999991118 ) ;
#18187 = PLANE ( 'NONE',  #7654 ) ;
#18188 = EDGE_CURVE ( 'NONE', #14057, #13289, #16467, .T. ) ;
#18189 = DIRECTION ( 'NONE',  ( 0.000000000000000000, 0.000000000000000000, 1.000000000000000000 ) ) ;
#18190 = CARTESIAN_POINT ( 'NONE',  ( -9.000000000000003553, 18.79999999999999361, -2.500000000000001776 ) ) ;
#18191 = EDGE_CURVE ( 'NONE', #5758, #4066, #14068, .T. ) ;
#18192 = CARTESIAN_POINT ( 'NONE',  ( 2.121784821875004390, -19.94344952681598926, -10.60795278932534558 ) ) ;
#18193 = EDGE_LOOP ( 'NONE', ( #11466, #8593, #5168, #546, #3587 ) ) ;
#18194 = EDGE_CURVE ( 'NONE', #7871, #5980, #11567, .T. ) ;
#18195 = DIRECTION ( 'NONE',  ( -1.000000000000000000, 0.000000000000000000, 4.336808689942021680E-16 ) ) ;
#18196 = EDGE_LOOP ( 'NONE', ( #8474, #6923, #16083, #5798, #690 ) ) ;
#18197 = CARTESIAN_POINT ( 'NONE',  ( 2.000000000000004441, -22.06819172071273272, -13.27464081153562425 ) ) ;
#18198 = CARTESIAN_POINT ( 'NONE',  ( 4.000000000000000000, 0.000000000000000000, 0.000000000000000000 ) ) ;
#18199 = FACE_OUTER_BOUND ( 'NONE', #3359, .T. ) ;
#18200 = AXIS2_PLACEMENT_3D ( 'NONE', #17310, #699, #3195 ) ;
#18201 = SURFACE_STYLE_USAGE ( .BOTH. , #15661 ) ;
#18202 = VERTEX_POINT ( 'NONE', #14592 ) ;
#18203 = EDGE_CURVE ( 'NONE', #17988, #5572, #16077, .T. ) ;
#18204 = CARTESIAN_POINT ( 'NONE',  ( 3.481649420246394122, 38.37819992234354771, 1.193696214020467439 ) ) ;
#18205 = CARTESIAN_POINT ( 'NONE',  ( 1.027846397803612311, 16.25319992234354416, 3.346150245485499219 ) ) ;
#18206 = CARTESIAN_POINT ( 'NONE',  ( 1.999999999999994449, -29.37813640364300127, -11.63537001862205855 ) ) ;
#18207 = CARTESIAN_POINT ( 'NONE',  ( 2.518350579753628971, 26.87180007765648426, 0.7558219633769073242 ) ) ;
#18208 = CARTESIAN_POINT ( 'NONE',  ( -4.499999999999999112, 29.50319992234354061, -0.05647727720528529505 ) ) ;
#18209 = CARTESIAN_POINT ( 'NONE',  ( 1.999999999999994449, -28.28117146841668728, -10.06874173291258856 ) ) ;
#18210 = VERTEX_POINT ( 'NONE', #3460 ) ;
#18211 = CARTESIAN_POINT ( 'NONE',  ( -5.330712181944245322E-15, -23.71987649689963362, -1.051034048512634156 ) ) ;
#18212 = CARTESIAN_POINT ( 'NONE',  ( 0.05938372350927906274, 22.37180007765648071, 3.680117784833935701 ) ) ;
#18213 = DIRECTION ( 'NONE',  ( 0.000000000000000000, 0.000000000000000000, 1.000000000000000000 ) ) ;
#18214 = CARTESIAN_POINT ( 'NONE',  ( 4.243569643749997233, -24.47685408073152402, -6.403600187652020104 ) ) ;
#18215 = CARTESIAN_POINT ( 'NONE',  ( 0.000000000000000000, 13.00000000000000178, 0.000000000000000000 ) ) ;
#18216 = CARTESIAN_POINT ( 'NONE',  ( 1.999999999999994449, -25.18385871212106863, -5.645320693752015728 ) ) ;
#18217 = DIRECTION ( 'NONE',  ( 0.000000000000000000, 0.000000000000000000, 1.000000000000000000 ) ) ;
#18218 = ORIENTED_EDGE ( 'NONE', *, *, #15742, .T. ) ;
#18219 = VERTEX_POINT ( 'NONE', #3180 ) ;
#18220 = FACE_OUTER_BOUND ( 'NONE', #12889, .T. ) ;
#18221 = CARTESIAN_POINT ( 'NONE',  ( 0.000000000000000000, 5.977523610840987267, 32.81826849749789687 ) ) ;
#18222 = CARTESIAN_POINT ( 'NONE',  ( 1.071796769724504328, -24.92302254597699118, -4.338497721120512907 ) ) ;
#18223 = ORIENTED_EDGE ( 'NONE', *, *, #6811, .F. ) ;
#18224 = CARTESIAN_POINT ( 'NONE',  ( 0.7188294034286553114, 38.75319992234354061, 2.395093729190349130 ) ) ;
#18225 = CARTESIAN_POINT ( 'NONE',  ( 2.121784821874994176, -27.56671030237578179, -8.680627135892345692 ) ) ;
#18226 = CARTESIAN_POINT ( 'NONE',  ( -0.05938372350927861171, 28.62180007765648071, -3.680117784833935701 ) ) ;
#18227 =( BOUNDED_CURVE ( )  B_SPLINE_CURVE ( 2, ( #15683, #10006, #2978, #11767, #102, #13162, #10090, #472, #10379 ),
 .UNSPECIFIED., .F., .F. ) 
 B_SPLINE_CURVE_WITH_KNOTS ( ( 3, 2, 2, 2, 3 ),
 ( 0.9568965517241379004, 0.9597701149425287293, 0.9655172413793103869, 0.9712643678160919336, 0.9741379310344827624 ),
 .UNSPECIFIED. ) 
 CURVE ( )  GEOMETRIC_REPRESENTATION_ITEM ( )  RATIONAL_B_SPLINE_CURVE ( ( 0.9330127018922194093, 0.9330127018922194093, 1.000000000000000000, 0.8660254037844387076, 1.000000000000000000, 0.8660254037844387076, 1.000000000000000000, 0.9330127018922194093, 0.9330127018922194093 ) ) 
 REPRESENTATION_ITEM ( '' )  );
#18228 = CARTESIAN_POINT ( 'NONE',  ( -1.135272562821019626, 26.50319992234354771, 3.311245368580577164 ) ) ;
#18229 = CARTESIAN_POINT ( 'NONE',  ( -1.734723475976807094E-15, 27.59999999999999432, -2.500000000000000000 ) ) ;
#18230 = DIRECTION ( 'NONE',  ( 0.000000000000000000, 0.8191520442889952403, -0.5735764363510411634 ) ) ;
#18231 = CARTESIAN_POINT ( 'NONE',  ( -4.243569643750000786, -23.90026645004723704, -9.851637823819498152 ) ) ;
#18232 = DIRECTION ( 'NONE',  ( 0.000000000000000000, 0.000000000000000000, 1.000000000000000000 ) ) ;
#18233 = FACE_OUTER_BOUND ( 'NONE', #4358, .T. ) ;
#18234 = CARTESIAN_POINT ( 'NONE',  ( -1.071796769724486786, -17.72453270077011922, -8.005563162103721098 ) ) ;
#18235 = CARTESIAN_POINT ( 'NONE',  ( 4.243569643750003451, -20.41994811033581314, -9.152718235773933841 ) ) ;
#18236 = EDGE_CURVE ( 'NONE', #1028, #1579, #4471, .T. ) ;
#18237 = CARTESIAN_POINT ( 'NONE',  ( -5.577813053751546416E-15, -25.19265864305380376, -4.723577975706471754 ) ) ;
#18238 = CARTESIAN_POINT ( 'NONE',  ( 2.500000000000001332, 15.75319992234354594, 0.05647727720530566764 ) ) ;
#18239 = CARTESIAN_POINT ( 'NONE',  ( -1.071796769724505882, -18.95055233276553608, -9.756500655764678953 ) ) ;
#18240 = CARTESIAN_POINT ( 'NONE',  ( 1.135272562821090458, 34.74680007765648071, 3.311245368580554072 ) ) ;
#18241 = DIRECTION ( 'NONE',  ( 1.000000000000000000, 0.000000000000000000, 0.000000000000000000 ) ) ;
#18242 = CONTEXT_DEPENDENT_SHAPE_REPRESENTATION ( #15200, #15089 ) ;
#18243 = CARTESIAN_POINT ( 'NONE',  ( 13.80999999999999872, 0.000000000000000000, 0.000000000000000000 ) ) ;
#18244 = ADVANCED_BREP_SHAPE_REPRESENTATION ( '', ( #7672, #7822, #7707, #13807, #2004, #1553, #14621, #8199, #13775, #8351, #14214, #14659, #2247, #16940 ), #11010 ) ;
#18245 = ORIENTED_EDGE ( 'NONE', *, *, #12602, .T. ) ;
#18246 = CARTESIAN_POINT ( 'NONE',  ( 4.243569643749997233, -23.21857077348643372, -4.606585390493036947 ) ) ;
#18247 = CARTESIAN_POINT ( 'NONE',  ( 3.518350579753631191, 29.37180007765647005, 1.080741659609802285 ) ) ;
#18248 =( BOUNDED_CURVE ( )  B_SPLINE_CURVE ( 2, ( #4279, #10096, #15778, #12981, #12620, #4191, #8440, #14109, #1420 ),
 .UNSPECIFIED., .F., .T. ) 
 B_SPLINE_CURVE_WITH_KNOTS ( ( 3, 2, 2, 2, 3 ),
 ( 0.7844827586206897241, 0.7873563218390804419, 0.7931034482758620996, 0.7988505747126436463, 0.8017241379310344751 ),
 .UNSPECIFIED. ) 
 CURVE ( )  GEOMETRIC_REPRESENTATION_ITEM ( )  RATIONAL_B_SPLINE_CURVE ( ( 0.9330127018922194093, 0.9330127018922206306, 1.000000000000000000, 0.8660254037844387076, 1.000000000000000000, 0.8660254037844387076, 1.000000000000000000, 0.9330127018922194093, 0.9330127018922194093 ) ) 
 REPRESENTATION_ITEM ( '' )  );
#18249 = DIRECTION ( 'NONE',  ( -1.000000000000000000, 0.000000000000000000, 4.336808689942021680E-16 ) ) ;
#18250 = CARTESIAN_POINT ( 'NONE',  ( -5.330712181944246111E-15, -30.91467592037800927, -11.32627250406271457 ) ) ;
#18251 = DIRECTION ( 'NONE',  ( 3.469446951953612217E-16, -0.000000000000000000, 1.000000000000000000 ) ) ;
#18252 = LINE ( 'NONE', #10996, #17493 ) ;
#18253 = EDGE_CURVE ( 'NONE', #6645, #4921, #10400, .T. ) ;
#18254 = CARTESIAN_POINT ( 'NONE',  ( -8.000000000000001776, 23.19999999999999574, 2.499999999999998224 ) ) ;
#18255 = CARTESIAN_POINT ( 'NONE',  ( -2.121784821874996396, -23.22358977219849407, -15.29247854260303718 ) ) ;
#18256 = VERTEX_POINT ( 'NONE', #8721 ) ;
#18257 = DIRECTION ( 'NONE',  ( -1.000000000000000000, 0.000000000000000000, 4.336808689942021680E-16 ) ) ;
#18258 = CARTESIAN_POINT ( 'NONE',  ( -4.000000000000000888, -21.46435902227137760, -6.372801486233056423 ) ) ;
#18259 = CARTESIAN_POINT ( 'NONE',  ( -2.798362969681365886, 40.24680007765648071, 2.102939460078824929 ) ) ;
#18260 = ORIENTED_EDGE ( 'NONE', *, *, #11239, .F. ) ;
#18261 = DIRECTION ( 'NONE',  ( -0.000000000000000000, -1.000000000000000000, -0.000000000000000000 ) ) ;
#18262 = CARTESIAN_POINT ( 'NONE',  ( 2.733110507866247652, 16.37180007765647716, -3.862833514489153686 ) ) ;
#18263 = UNCERTAINTY_MEASURE_WITH_UNIT (LENGTH_MEASURE( 1.000000000000000082E-05 ), #2338, 'distance_accuracy_value', 'NONE');
#18264 = CARTESIAN_POINT ( 'NONE',  ( 4.000000000000003553, -21.68050181204657889, -10.70780328770074696 ) ) ;
#18265 = CARTESIAN_POINT ( 'NONE',  ( 1.989345975306457071, 33.50319992234354061, 1.515154207786300500 ) ) ;
#18266 = VERTEX_POINT ( 'NONE', #11693 ) ;
#18267 = CARTESIAN_POINT ( 'NONE',  ( 2.121784821875004390, -22.00832469767973620, -13.55690014876572569 ) ) ;
#18268 = CARTESIAN_POINT ( 'NONE',  ( -2.829195390882805139, 23.37180007765647716, -3.793023760679206102 ) ) ;
#18269 = VECTOR ( 'NONE', #2421, 1000.000000000000000 ) ;
#18270 = ORIENTED_EDGE ( 'NONE', *, *, #1449, .F. ) ;
#18271 = CARTESIAN_POINT ( 'NONE',  ( 0.000000000000000000, 4.000000000000007105, 4.000000000000000000 ) ) ;
#18272 = CARTESIAN_POINT ( 'NONE',  ( 0.000000000000000000, 10.00000000000000000, 0.000000000000000000 ) ) ;
#18273 = CARTESIAN_POINT ( 'NONE',  ( -8.500000000000007105, 15.00000000000000000, -22.69999999999999929 ) ) ;
#18274 = CARTESIAN_POINT ( 'NONE',  ( 2.121784821874994176, -25.27598940969881269, -5.409138659013170702 ) ) ;
#18275 = ORIENTED_EDGE ( 'NONE', *, *, #9603, .F. ) ;
#18276 = CARTESIAN_POINT ( 'NONE',  ( 14.20000000000000107, 0.000000000000000000, 1.610000000000000098 ) ) ;
#18277 = ORIENTED_EDGE ( 'NONE', *, *, #2644, .F. ) ;
#18278 = TOROIDAL_SURFACE ( 'NONE', #1088, 9.000000000000001776, 0.9999999999999991118 ) ;
#18279 = CARTESIAN_POINT ( 'NONE',  ( 4.713407268011036227E-15, -20.84269790143662959, -13.53761320980093785 ) ) ;
#18280 = LINE ( 'NONE', #16799, #12193 ) ;
#18281 = CYLINDRICAL_SURFACE ( 'NONE', #7468, 2.000000000000001776 ) ;
#18282 = APPLICATION_PROTOCOL_DEFINITION ( 'draft international standard', 'automotive_design', 1998, #8188 ) ;
#18283 = CARTESIAN_POINT ( 'NONE',  ( -4.518350579753602325, 19.37819992234354061, 1.405661355842794391 ) ) ;
#18284 = CARTESIAN_POINT ( 'NONE',  ( -3.500000000000000444, 22.00319992234354416, -0.05647727720529563400 ) ) ;
#18285 = CARTESIAN_POINT ( 'NONE',  ( 1.999999999999994449, -28.60380821456909572, -10.52951475883191357 ) ) ;
#18286 = CARTESIAN_POINT ( 'NONE',  ( 2.518350579753611207, 15.62819992234354594, -0.7558219633769606149 ) ) ;
#18287 = EDGE_CURVE ( 'NONE', #985, #8838, #3148, .T. ) ;
#18288 = CARTESIAN_POINT ( 'NONE',  ( 2.733110507866328920, 23.62819992234354416, 3.862833514489095510 ) ) ;
#18289 = EDGE_CURVE ( 'NONE', #11559, #1834, #6134, .T. ) ;
#18290 = UNCERTAINTY_MEASURE_WITH_UNIT (LENGTH_MEASURE( 1.000000000000000082E-05 ), #7674, 'distance_accuracy_value', 'NONE');
#18291 = CARTESIAN_POINT ( 'NONE',  ( 4.000000000000000888, -23.33565214516171338, -9.045285029719133618 ) ) ;
#18292 = ORIENTED_EDGE ( 'NONE', *, *, #14355, .F. ) ;
#18293 = EDGE_CURVE ( 'NONE', #7975, #723, #11785, .T. ) ;
#18294 = CARTESIAN_POINT ( 'NONE',  ( -5.330712181944245322E-15, -23.97798589325759977, -1.419652468442682558 ) ) ;
#18295 = VECTOR ( 'NONE', #12062, 1000.000000000000000 ) ;
#18296 = CARTESIAN_POINT ( 'NONE',  ( -1.135272562821090014, 20.99680007765647716, -3.311245368580554072 ) ) ;
#18297 = DIRECTION ( 'NONE',  ( 0.000000000000000000, 0.8191520442889952403, -0.5735764363510413855 ) ) ;
#18298 = ADVANCED_FACE ( 'NONE', ( #1989 ), #5949, .F. ) ;
#18299 = CARTESIAN_POINT ( 'NONE',  ( 4.243569643750000786, -23.22272928460757413, -8.884014471503119736 ) ) ;
#18300 = DIRECTION ( 'NONE',  ( -0.000000000000000000, 0.8660254037844391517, 0.4999999999999990563 ) ) ;
#18301 = CARTESIAN_POINT ( 'NONE',  ( -5.577813053751546416E-15, -23.38589286854802296, -2.143249036196138047 ) ) ;
#18302 = DIRECTION ( 'NONE',  ( 0.000000000000000000, 0.000000000000000000, 1.000000000000000000 ) ) ;
#18303 = ORIENTED_EDGE ( 'NONE', *, *, #15380, .F. ) ;
#18304 = ORIENTED_EDGE ( 'NONE', *, *, #3829, .T. ) ;
#18305 = CARTESIAN_POINT ( 'NONE',  ( -2.864755990943265829, 25.74680007765647716, -2.011557305968488141 ) ) ;
#18306 = DIRECTION ( 'NONE',  ( 0.000000000000000000, -1.000000000000000000, 0.000000000000000000 ) ) ;
#18307 = CARTESIAN_POINT ( 'NONE',  ( -4.000000000000004441, -27.98056965346157554, -11.65259680360068018 ) ) ;
#18308 = CARTESIAN_POINT ( 'NONE',  ( -3.999999999999997335, -22.62690293202579284, -12.05940416077759103 ) ) ;
#18309 = CARTESIAN_POINT ( 'NONE',  ( 1.071796769724485232, -26.21356952776684679, -6.181589820770747146 ) ) ;
#18310 = VERTEX_POINT ( 'NONE', #7613 ) ;
#18311 = AXIS2_PLACEMENT_3D ( 'NONE', #13666, #2563, #16660 ) ;
#18312 = CARTESIAN_POINT ( 'NONE',  ( 1.027846397803612311, 18.75319992234354771, 3.346150245485499219 ) ) ;
#18313 = CIRCLE ( 'NONE', #4951, 2.149999999999995470 ) ;
#18314 = CARTESIAN_POINT ( 'NONE',  ( -2.121784821874996396, -20.12627701590287543, -10.86905750344246435 ) ) ;
#18315 = CARTESIAN_POINT ( 'NONE',  ( -1.135272562821090014, 28.49680007765648071, -3.311245368580554072 ) ) ;
#18316 = CARTESIAN_POINT ( 'NONE',  ( 1.135272562821020070, 25.25319992234354416, -3.311245368580577164 ) ) ;
#18317 = LINE ( 'NONE', #11235, #4018 ) ;
#18318 = CYLINDRICAL_SURFACE ( 'NONE', #15881, 0.9999999999999991118 ) ;
#18319 = CARTESIAN_POINT ( 'NONE',  ( -2.121784821874996396, -20.67475948316355883, -11.65237164579381535 ) ) ;
#18320 = AXIS2_PLACEMENT_3D ( 'NONE', #9983, #3138, #7205 ) ;
#18321 = AXIS2_PLACEMENT_3D ( 'NONE', #3745, #982, #10884 ) ;
#18322 = DIRECTION ( 'NONE',  ( 0.000000000000000000, -1.000000000000000000, 0.000000000000000000 ) ) ;
#18323 = LINE ( 'NONE', #16748, #5325 ) ;
#18324 = DIRECTION ( 'NONE',  ( 0.000000000000000000, 0.000000000000000000, 1.000000000000000000 ) ) ;
#18325 =( BOUNDED_CURVE ( )  B_SPLINE_CURVE ( 2, ( #11455, #7010, #5728, #17343, #17148, #2952, #17245, #12679, #5904 ),
 .UNSPECIFIED., .F., .F. ) 
 B_SPLINE_CURVE_WITH_KNOTS ( ( 3, 2, 2, 2, 3 ),
 ( 0.7844827586206897241, 0.7873563218390804419, 0.7931034482758620996, 0.7988505747126436463, 0.8017241379310344751 ),
 .UNSPECIFIED. ) 
 CURVE ( )  GEOMETRIC_REPRESENTATION_ITEM ( )  RATIONAL_B_SPLINE_CURVE ( ( 0.9330127018922194093, 0.9330127018922206306, 1.000000000000000000, 0.8660254037844387076, 1.000000000000000000, 0.8660254037844387076, 1.000000000000000000, 0.9330127018922194093, 0.9330127018922194093 ) ) 
 REPRESENTATION_ITEM ( '' )  );
#18326 = CARTESIAN_POINT ( 'NONE',  ( -4.243569643750000786, -20.77069001920686375, -5.382139482167671574 ) ) ;
#18327 = CYLINDRICAL_SURFACE ( 'NONE', #8558, 4.000000000000000000 ) ;
#18328 = FACE_OUTER_BOUND ( 'NONE', #14505, .T. ) ;
#18329 = ORIENTED_EDGE ( 'NONE', *, *, #11981, .T. ) ;
#18330 = EDGE_CURVE ( 'NONE', #5909, #904, #591, .T. ) ;
#18331 = CARTESIAN_POINT ( 'NONE',  ( -2.500000000000001332, 37.99680007765646650, 0.05647727720535858364 ) ) ;
#18332 = CARTESIAN_POINT ( 'NONE',  ( 4.243569643750003451, -24.54969845206331058, -15.05061295465469762 ) ) ;
#18333 = CARTESIAN_POINT ( 'NONE',  ( 3.518350579753631191, 36.87180007765647360, 1.080741659609802729 ) ) ;
#18334 = TOROIDAL_SURFACE ( 'NONE', #10603, 2.200000000000000178, 0.2000000000000000111 ) ;
#18335 = CARTESIAN_POINT ( 'NONE',  ( -9.996898113758209803, -9.916603943890297757, 4.932537101542136426 ) ) ;
#18336 = AXIS2_PLACEMENT_3D ( 'NONE', #13927, #15589, #18030 ) ;
#18337 = ORIENTED_EDGE ( 'NONE', *, *, #16585, .T. ) ;
#18338 = LINE ( 'NONE', #14134, #6083 ) ;
#18339 = CARTESIAN_POINT ( 'NONE',  ( -3.518350579753630747, 33.12180007765646650, -1.080741659609802729 ) ) ;
#18340 = CARTESIAN_POINT ( 'NONE',  ( 0.000000000000000000, 27.59999999999999432, 2.500000000000000000 ) ) ;
#18341 = CARTESIAN_POINT ( 'NONE',  ( -2.121784821874996396, -23.99791796127240318, -16.39833380239318217 ) ) ;
#18342 = AXIS2_PLACEMENT_3D ( 'NONE', #3753, #15357, #16845 ) ;
#18343 = DIRECTION ( 'NONE',  ( -0.000000000000000000, 1.000000000000000000, -0.000000000000000000 ) ) ;
#18344 = FACE_OUTER_BOUND ( 'NONE', #10674, .T. ) ;
#18346 = CARTESIAN_POINT ( 'NONE',  ( 4.898587196589413815E-16, 2.700915433685006750, 35.11257424290206330 ) ) ;
#18345 = AXIS2_PLACEMENT_3D ( 'NONE', #11022, #16616, #18195 ) ;
#18347 = CARTESIAN_POINT ( 'NONE',  ( -2.121784821874996396, -22.96548037584052793, -14.92386012267298945 ) ) ;
#18348 = ORIENTED_EDGE ( 'NONE', *, *, #11410, .T. ) ;
#18349 = CARTESIAN_POINT ( 'NONE',  ( -8.000000000000003553, 36.39999999999999147, -2.500000000000001776 ) ) ;
#18350 = CARTESIAN_POINT ( 'NONE',  ( -4.000000000000000888, -22.23868721134528670, -7.478656746023200519 ) ) ;
#18351 = CARTESIAN_POINT ( 'NONE',  ( -1.593127413382998459, 15.87180007765648071, -2.091722143975139669 ) ) ;
#18352 = VERTEX_POINT ( 'NONE', #7241 ) ;
#18353 = CARTESIAN_POINT ( 'NONE',  ( 6.123233995736766282E-16, 15.00000000000000355, -5.000000000000000000 ) ) ;
#18354 = EDGE_CURVE ( 'NONE', #13234, #12374, #3897, .T. ) ;
#18355 = LINE ( 'NONE', #15733, #14009 ) ;
#18356 = CARTESIAN_POINT ( 'NONE',  ( -0.8262555684460826111, 34.00319992234354771, 2.360188852285421302 ) ) ;
#18357 = ADVANCED_FACE ( 'NONE', ( #12900 ), #7527, .F. ) ;
#18358 = ORIENTED_EDGE ( 'NONE', *, *, #684, .T. ) ;
#18359 = CARTESIAN_POINT ( 'NONE',  ( -4.243569643749998122, -23.72159747208148772, -13.86796219071246483 ) ) ;
#18360 = CIRCLE ( 'NONE', #6183, 10.00000000000000178 ) ;
#18361 = CARTESIAN_POINT ( 'NONE',  ( -2.733110507866247652, 35.12180007765647360, 3.862833514489154574 ) ) ;
#18363 = ADVANCED_FACE ( 'NONE', ( #17296 ), #208, .F. ) ;
#18362 = AXIS2_PLACEMENT_3D ( 'NONE', #10927, #10745, #11014 ) ;
#18364 = EDGE_LOOP ( 'NONE', ( #13774, #14957, #16592, #13530 ) ) ;
#18365 = CARTESIAN_POINT ( 'NONE',  ( 2.343145750507617642, 4.000000000000004441, 3.999999999999997335 ) ) ;
#18366 = SURFACE_STYLE_FILL_AREA ( #1111 ) ;
#18367 = CARTESIAN_POINT ( 'NONE',  ( 8.000000000000000000, 0.000000000000000000, 0.000000000000000000 ) ) ;
#18368 = CARTESIAN_POINT ( 'NONE',  ( -9.000000000000003553, 16.59999999999999787, -2.500000000000001776 ) ) ;
#18369 = CARTESIAN_POINT ( 'NONE',  ( -0.05938372350926768989, 38.62180007765647360, -2.628655560595669183 ) ) ;
#18370 = NEXT_ASSEMBLY_USAGE_OCCURRENCE ( 'NAUO1', ' ', ' ', #13528, #3009, $ ) ;
#18371 = NEXT_ASSEMBLY_USAGE_OCCURRENCE ( 'NAUO2', ' ', ' ', #13528, #13870, $ ) ;
#18372 = NEXT_ASSEMBLY_USAGE_OCCURRENCE ( 'NAUO3', ' ', ' ', #13528, #2104, $ ) ;
#18373 = NEXT_ASSEMBLY_USAGE_OCCURRENCE ( 'NAUO4', ' ', ' ', #13528, #6725, $ ) ;
#18374 = NEXT_ASSEMBLY_USAGE_OCCURRENCE ( 'NAUO5', ' ', ' ', #13528, #16042, $ ) ;
#18375 = NEXT_ASSEMBLY_USAGE_OCCURRENCE ( 'NAUO6', ' ', ' ', #13528, #11945, $ ) ;
#18376 = NEXT_ASSEMBLY_USAGE_OCCURRENCE ( 'NAUO7', ' ', ' ', #13528, #2334, $ ) ;
#18377 = NEXT_ASSEMBLY_USAGE_OCCURRENCE ( 'NAUO8', ' ', ' ', #13528, #5599, $ ) ;
#18378 = NEXT_ASSEMBLY_USAGE_OCCURRENCE ( 'NAUO9', ' ', ' ', #13528, #12171, $ ) ;
#18379 = NEXT_ASSEMBLY_USAGE_OCCURRENCE ( 'NAUO10', ' ', ' ', #13528, #12171, $ ) ;
#18380 = NEXT_ASSEMBLY_USAGE_OCCURRENCE ( 'NAUO11', ' ', ' ', #13528, #12171, $ ) ;
#18381 = NEXT_ASSEMBLY_USAGE_OCCURRENCE ( 'NAUO12', ' ', ' ', #13528, #12171, $ ) ;
#18382 = NEXT_ASSEMBLY_USAGE_OCCURRENCE ( 'NAUO13', ' ', ' ', #13528, #155, $ ) ;
#18383=COLOUR_RGB('Dark Blue',0.08,0.2,0.34);
#18384=FILL_AREA_STYLE_COLOUR('',#18383);
#18385=FILL_AREA_STYLE('',(#18384));
#18386=SURFACE_STYLE_FILL_AREA(#18385);
#18387=SURFACE_SIDE_STYLE('',(#18386));
#18388=SURFACE_STYLE_USAGE(.BOTH.,#18387);
#18389=PRESENTATION_STYLE_ASSIGNMENT((#18388));
#18390=COLOUR_RGB('Light Blue',0.38,0.62,0.78);
#18391=FILL_AREA_STYLE_COLOUR('',#18390);
#18392=FILL_AREA_STYLE('',(#18391));
#18393=SURFACE_STYLE_FILL_AREA(#18392);
#18394=SURFACE_SIDE_STYLE('',(#18393));
#18395=SURFACE_STYLE_USAGE(.BOTH.,#18394);
#18396=PRESENTATION_STYLE_ASSIGNMENT((#18395));
#18397=COLOUR_RGB('Sky Blue',0.24,0.69,0.87);
#18398=FILL_AREA_STYLE_COLOUR('',#18397);
#18399=FILL_AREA_STYLE('',(#18398));
#18400=SURFACE_STYLE_FILL_AREA(#18399);
#18401=SURFACE_SIDE_STYLE('',(#18400));
#18402=SURFACE_STYLE_USAGE(.BOTH.,#18401);
#18403=PRESENTATION_STYLE_ASSIGNMENT((#18402));
#18404=COLOUR_RGB('Grey',0.48,0.52,0.57);
#18405=FILL_AREA_STYLE_COLOUR('',#18404);
#18406=FILL_AREA_STYLE('',(#18405));
#18407=SURFACE_STYLE_FILL_AREA(#18406);
#18408=SURFACE_SIDE_STYLE('',(#18407));
#18409=SURFACE_STYLE_USAGE(.BOTH.,#18408);
#18410=PRESENTATION_STYLE_ASSIGNMENT((#18409));
#18411=COLOUR_RGB('Black',0.12,0.14,0.17);
#18412=FILL_AREA_STYLE_COLOUR('',#18411);
#18413=FILL_AREA_STYLE('',(#18412));
#18414=SURFACE_STYLE_FILL_AREA(#18413);
#18415=SURFACE_SIDE_STYLE('',(#18414));
#18416=SURFACE_STYLE_USAGE(.BOTH.,#18415);
#18417=PRESENTATION_STYLE_ASSIGNMENT((#18416));
#18418=COLOUR_RGB('Off White',0.89,0.88,0.83);
#18419=FILL_AREA_STYLE_COLOUR('',#18418);
#18420=FILL_AREA_STYLE('',(#18419));
#18421=SURFACE_STYLE_FILL_AREA(#18420);
#18422=SURFACE_SIDE_STYLE('',(#18421));
#18423=SURFACE_STYLE_USAGE(.BOTH.,#18422);
#18424=PRESENTATION_STYLE_ASSIGNMENT((#18423));
ENDSEC;
END-ISO-10303-21;
